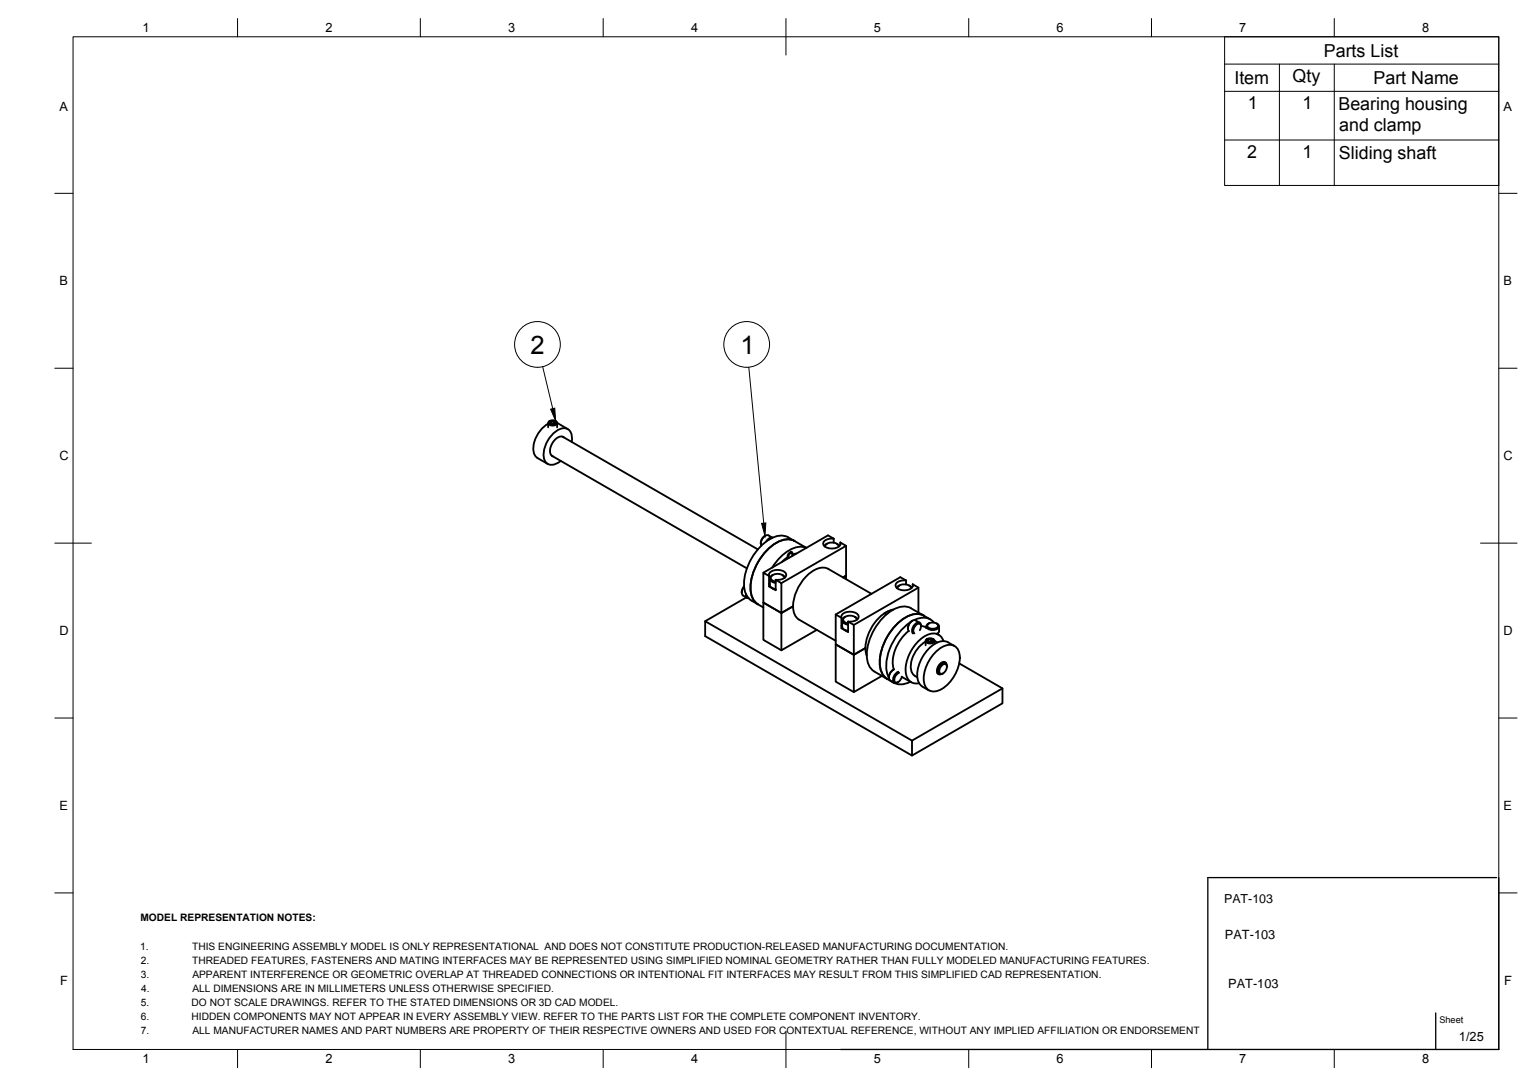
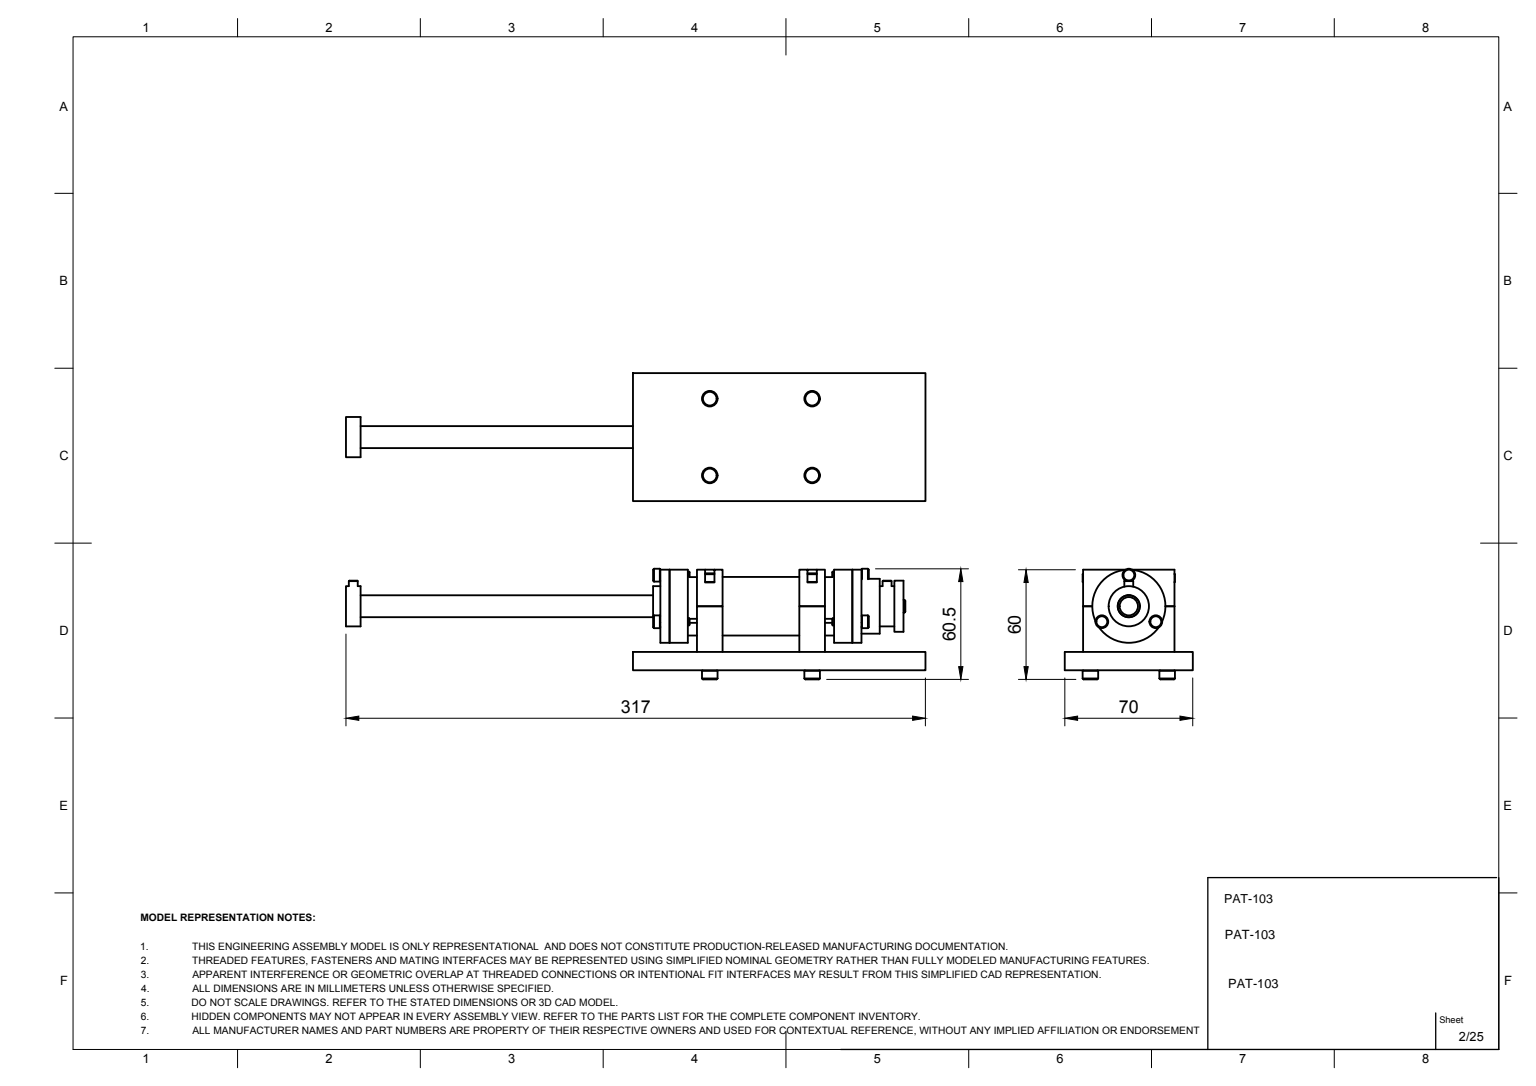
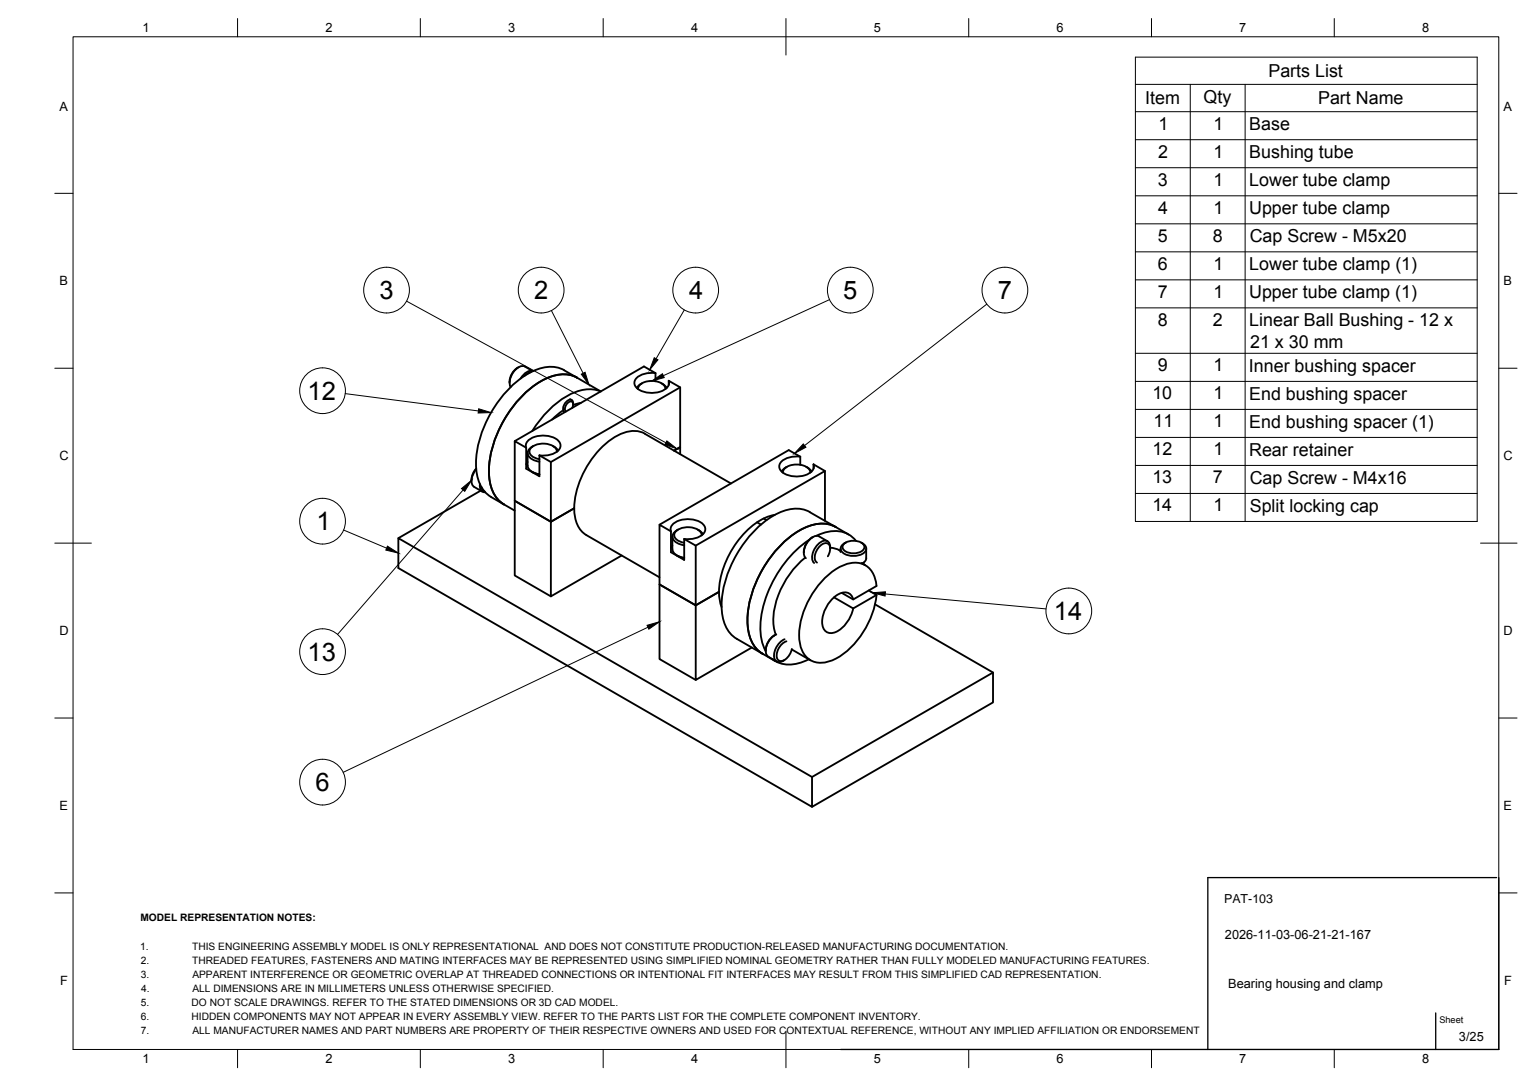
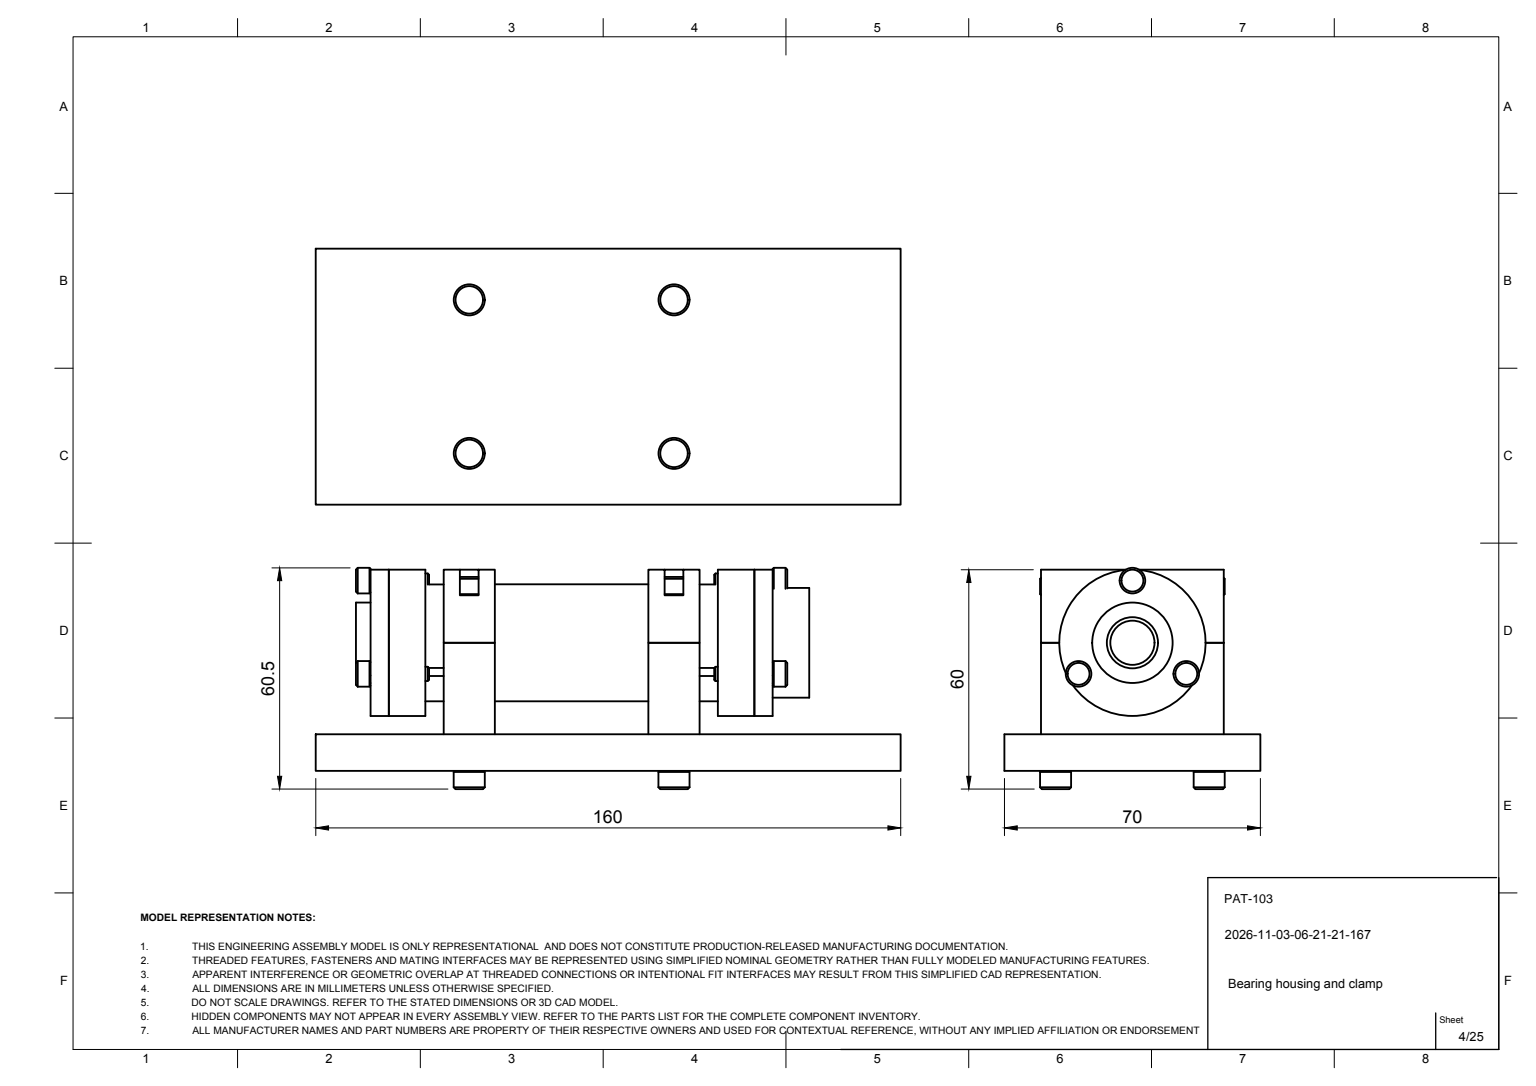
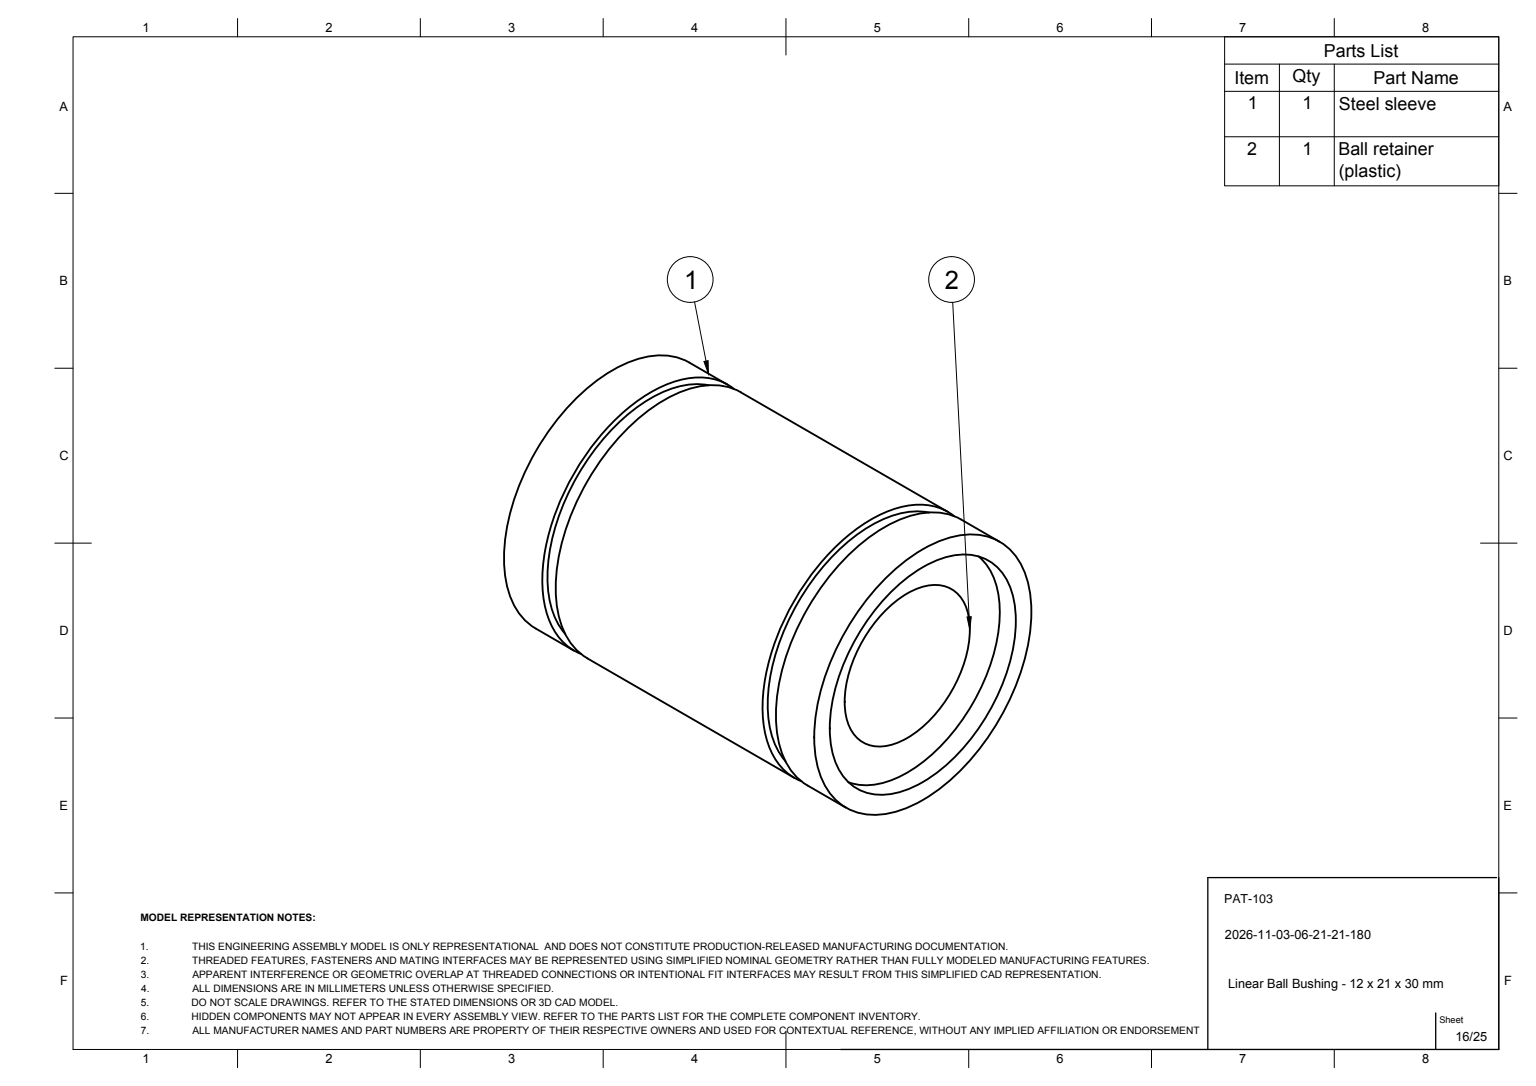
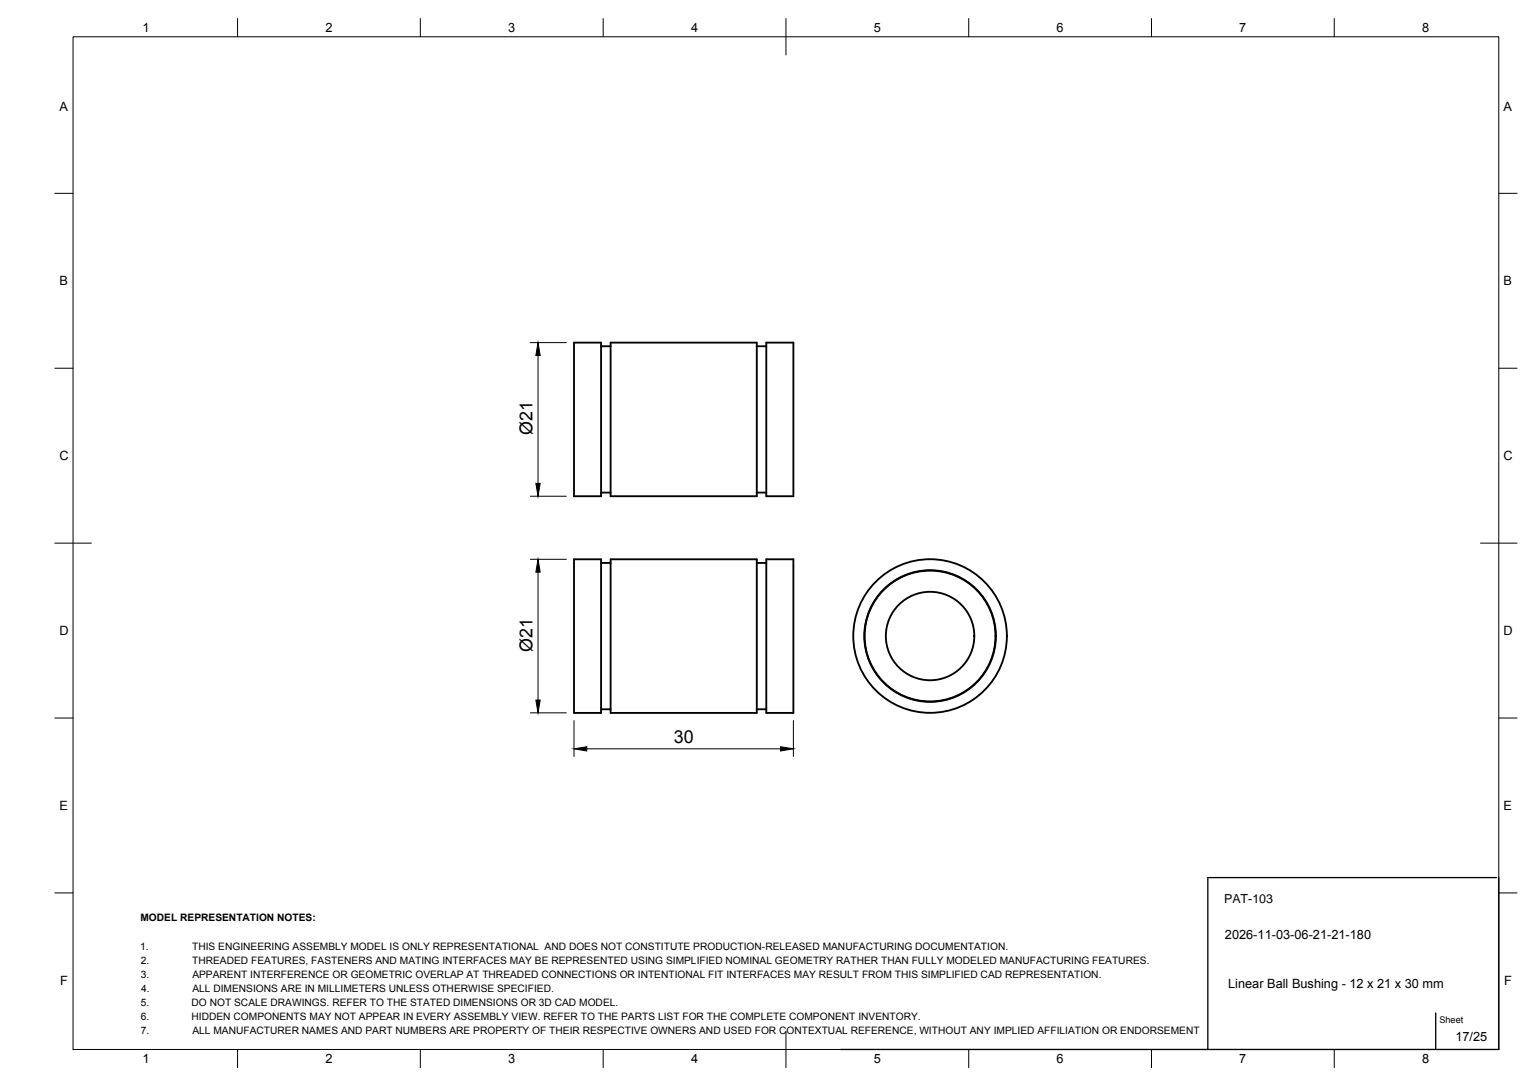
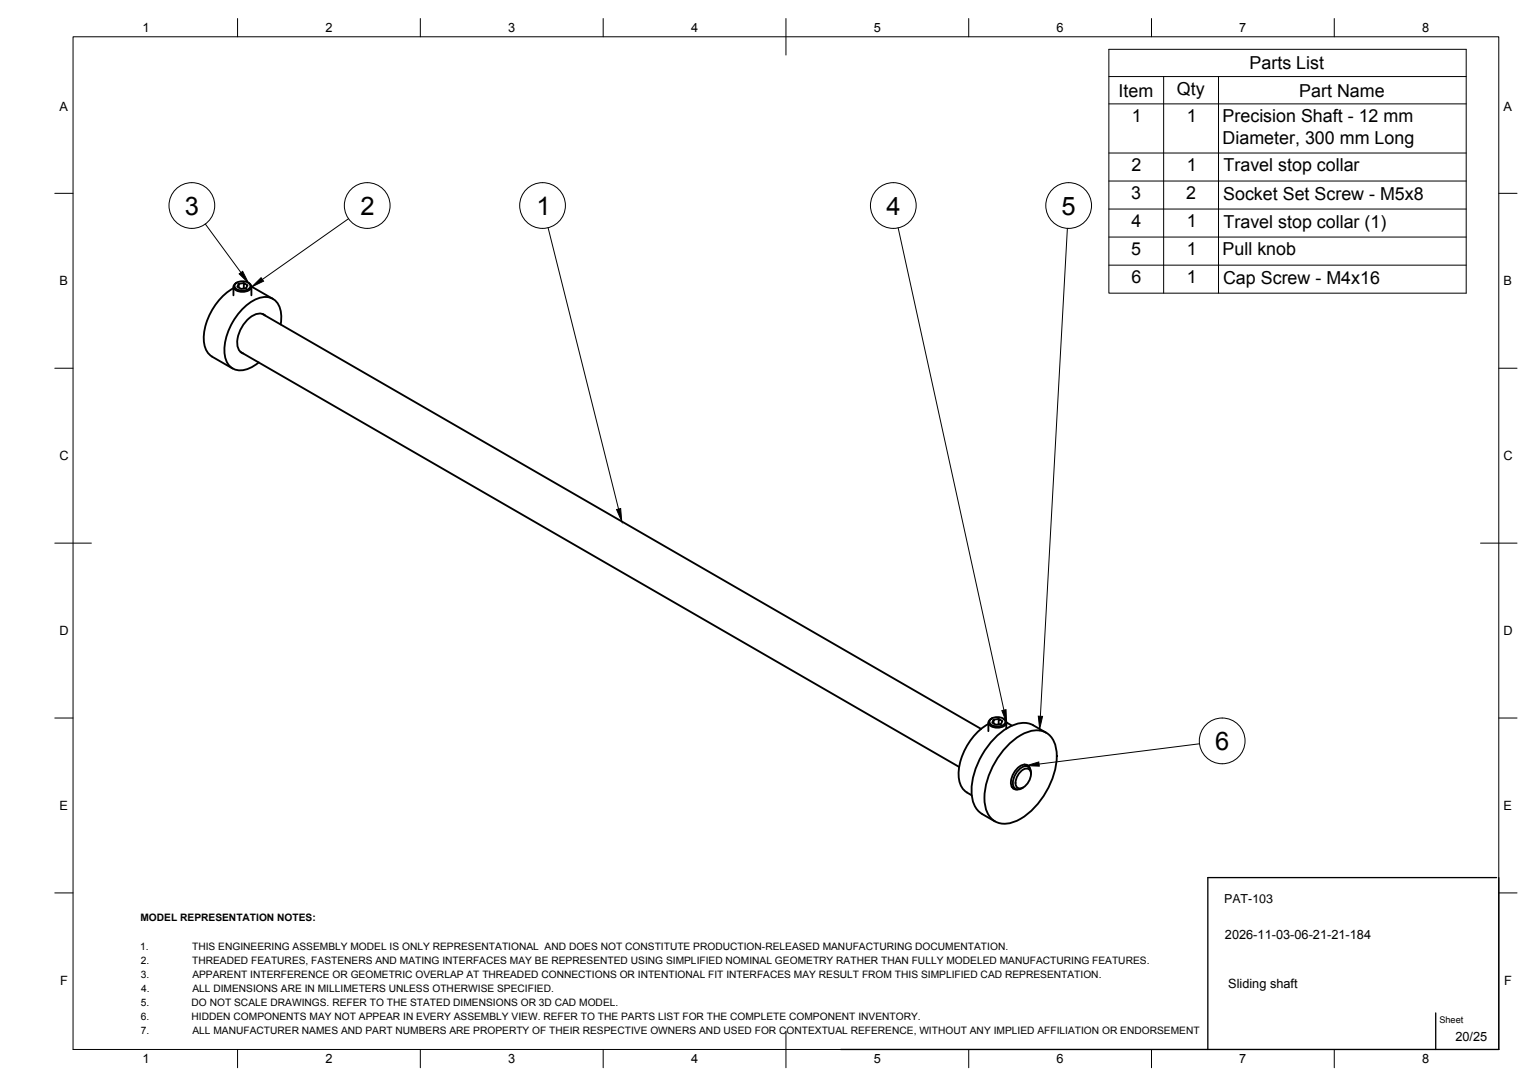
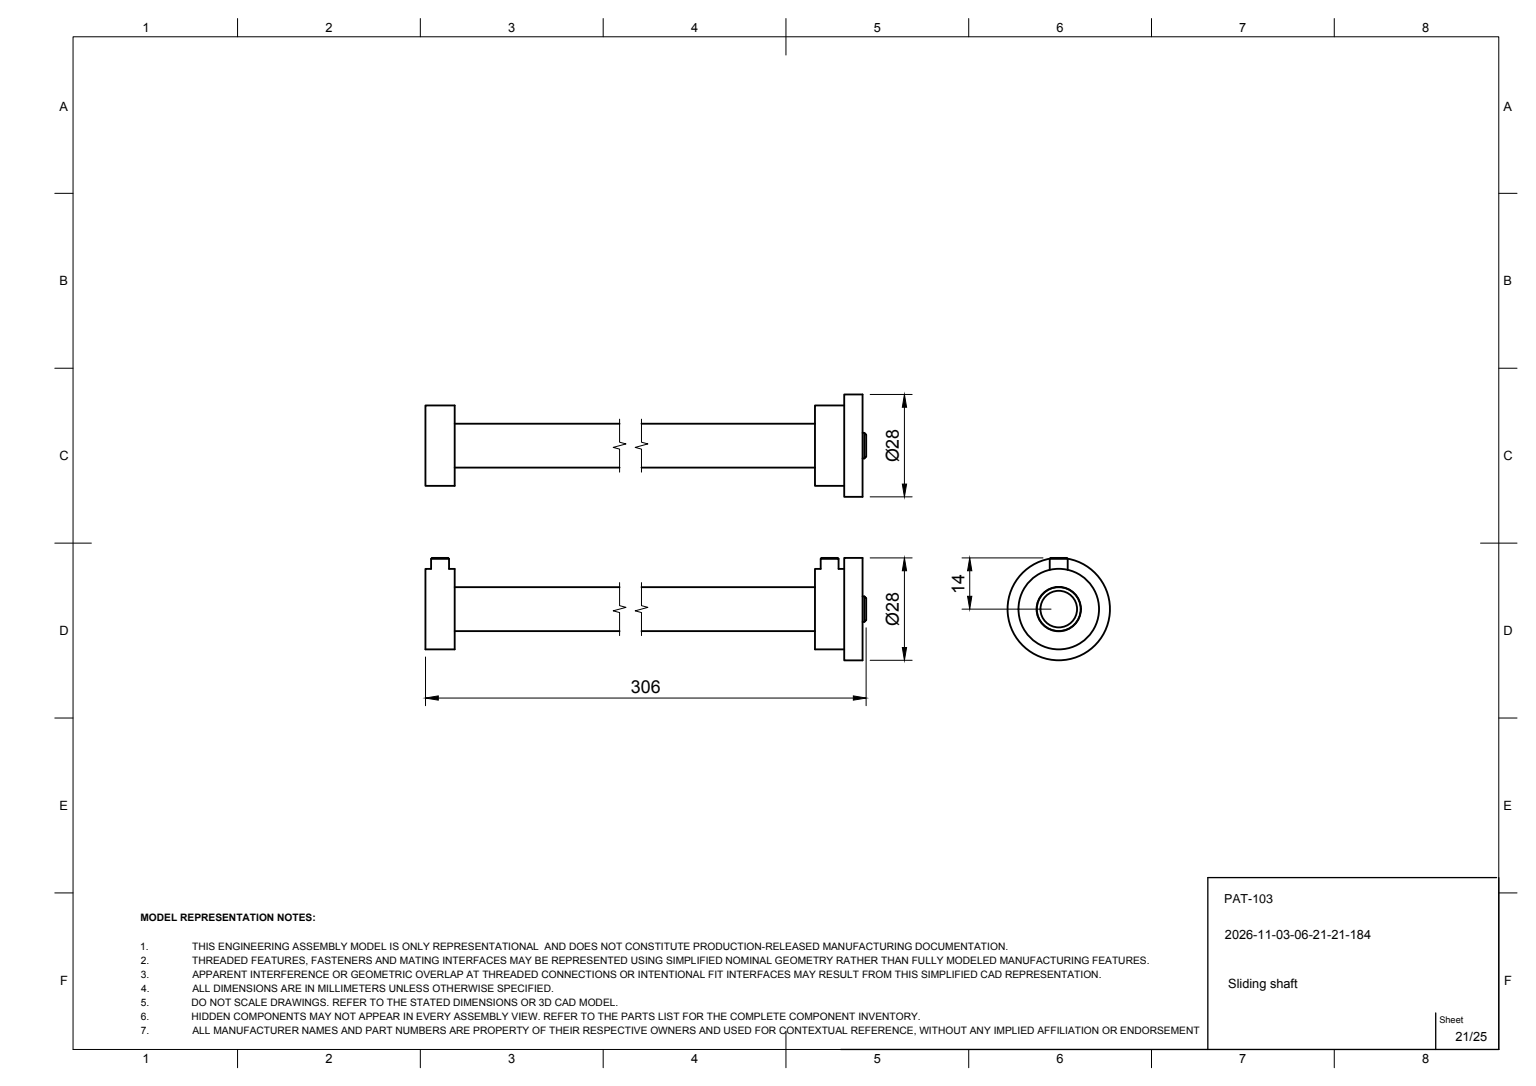
ISO-10303-21;
HEADER;
/* Generated by software containing ST-Developer
 * from STEP Tools, Inc. (www.steptools.com) 
 */

FILE_DESCRIPTION(
/* description */ ('Telescoping shaft support with lock collar'),
/* implementation_level */ '2;1');

FILE_NAME(
/* name */ 'PAT-103',
/* time_stamp */ '2026-10-27T10:48:51-07:00',
/* author */ (''),
/* organization */ (''),
/* preprocessor_version */ 'ST-DEVELOPER v20.2',
/* originating_system */ 'Autodesk Translation Framework v15.17.0.0',
/* authorisation */ '');

FILE_SCHEMA (('AUTOMOTIVE_DESIGN { 1 0 10303 214 3 1 1 }'));
ENDSEC;

DATA;
#10=MECHANICAL_DESIGN_GEOMETRIC_PRESENTATION_REPRESENTATION('',(#241,#242,
#243,#244,#245,#246,#247,#248,#249,#250,#251,#252,#253,#254,#255,#256,#257,
#258,#259,#260),#7349);
#11=ITEM_DEFINED_TRANSFORMATION($,$,#4520,#4569);
#12=ITEM_DEFINED_TRANSFORMATION($,$,#4552,#4570);
#13=ITEM_DEFINED_TRANSFORMATION($,$,#4209,#4670);
#14=ITEM_DEFINED_TRANSFORMATION($,$,#4228,#4671);
#15=ITEM_DEFINED_TRANSFORMATION($,$,#4293,#4672);
#16=ITEM_DEFINED_TRANSFORMATION($,$,#4320,#4673);
#17=ITEM_DEFINED_TRANSFORMATION($,$,#4345,#4674);
#18=ITEM_DEFINED_TRANSFORMATION($,$,#4372,#4675);
#19=ITEM_DEFINED_TRANSFORMATION($,$,#4397,#4676);
#20=ITEM_DEFINED_TRANSFORMATION($,$,#4406,#4677);
#21=ITEM_DEFINED_TRANSFORMATION($,$,#4415,#4678);
#22=ITEM_DEFINED_TRANSFORMATION($,$,#4424,#4679);
#23=ITEM_DEFINED_TRANSFORMATION($,$,#4446,#4680);
#24=ITEM_DEFINED_TRANSFORMATION($,$,#4493,#4681);
#25=ITEM_DEFINED_TRANSFORMATION($,$,#4493,#4682);
#26=ITEM_DEFINED_TRANSFORMATION($,$,#4493,#4683);
#27=ITEM_DEFINED_TRANSFORMATION($,$,#4493,#4684);
#28=ITEM_DEFINED_TRANSFORMATION($,$,#4493,#4685);
#29=ITEM_DEFINED_TRANSFORMATION($,$,#4493,#4686);
#30=ITEM_DEFINED_TRANSFORMATION($,$,#4493,#4687);
#31=ITEM_DEFINED_TRANSFORMATION($,$,#4493,#4688);
#32=ITEM_DEFINED_TRANSFORMATION($,$,#4519,#4689);
#33=ITEM_DEFINED_TRANSFORMATION($,$,#4519,#4690);
#34=ITEM_DEFINED_TRANSFORMATION($,$,#4644,#4691);
#35=ITEM_DEFINED_TRANSFORMATION($,$,#4644,#4692);
#36=ITEM_DEFINED_TRANSFORMATION($,$,#4644,#4693);
#37=ITEM_DEFINED_TRANSFORMATION($,$,#4644,#4694);
#38=ITEM_DEFINED_TRANSFORMATION($,$,#4644,#4695);
#39=ITEM_DEFINED_TRANSFORMATION($,$,#4644,#4696);
#40=ITEM_DEFINED_TRANSFORMATION($,$,#4644,#4697);
#41=ITEM_DEFINED_TRANSFORMATION($,$,#4572,#4698);
#42=ITEM_DEFINED_TRANSFORMATION($,$,#4586,#4699);
#43=ITEM_DEFINED_TRANSFORMATION($,$,#4600,#4700);
#44=ITEM_DEFINED_TRANSFORMATION($,$,#4613,#4701);
#45=ITEM_DEFINED_TRANSFORMATION($,$,#4627,#4702);
#46=ITEM_DEFINED_TRANSFORMATION($,$,#4627,#4703);
#47=ITEM_DEFINED_TRANSFORMATION($,$,#4644,#4704);
#48=ITEM_DEFINED_TRANSFORMATION($,$,#4208,#4705);
#49=ITEM_DEFINED_TRANSFORMATION($,$,#4571,#4706);
#50=(
REPRESENTATION_RELATIONSHIP($,$,#7456,#7455)
REPRESENTATION_RELATIONSHIP_WITH_TRANSFORMATION(#11)
SHAPE_REPRESENTATION_RELATIONSHIP()
);
#51=(
REPRESENTATION_RELATIONSHIP($,$,#7457,#7455)
REPRESENTATION_RELATIONSHIP_WITH_TRANSFORMATION(#12)
SHAPE_REPRESENTATION_RELATIONSHIP()
);
#52=(
REPRESENTATION_RELATIONSHIP($,$,#7443,#7442)
REPRESENTATION_RELATIONSHIP_WITH_TRANSFORMATION(#13)
SHAPE_REPRESENTATION_RELATIONSHIP()
);
#53=(
REPRESENTATION_RELATIONSHIP($,$,#7444,#7442)
REPRESENTATION_RELATIONSHIP_WITH_TRANSFORMATION(#14)
SHAPE_REPRESENTATION_RELATIONSHIP()
);
#54=(
REPRESENTATION_RELATIONSHIP($,$,#7445,#7442)
REPRESENTATION_RELATIONSHIP_WITH_TRANSFORMATION(#15)
SHAPE_REPRESENTATION_RELATIONSHIP()
);
#55=(
REPRESENTATION_RELATIONSHIP($,$,#7446,#7442)
REPRESENTATION_RELATIONSHIP_WITH_TRANSFORMATION(#16)
SHAPE_REPRESENTATION_RELATIONSHIP()
);
#56=(
REPRESENTATION_RELATIONSHIP($,$,#7447,#7442)
REPRESENTATION_RELATIONSHIP_WITH_TRANSFORMATION(#17)
SHAPE_REPRESENTATION_RELATIONSHIP()
);
#57=(
REPRESENTATION_RELATIONSHIP($,$,#7448,#7442)
REPRESENTATION_RELATIONSHIP_WITH_TRANSFORMATION(#18)
SHAPE_REPRESENTATION_RELATIONSHIP()
);
#58=(
REPRESENTATION_RELATIONSHIP($,$,#7449,#7442)
REPRESENTATION_RELATIONSHIP_WITH_TRANSFORMATION(#19)
SHAPE_REPRESENTATION_RELATIONSHIP()
);
#59=(
REPRESENTATION_RELATIONSHIP($,$,#7450,#7442)
REPRESENTATION_RELATIONSHIP_WITH_TRANSFORMATION(#20)
SHAPE_REPRESENTATION_RELATIONSHIP()
);
#60=(
REPRESENTATION_RELATIONSHIP($,$,#7451,#7442)
REPRESENTATION_RELATIONSHIP_WITH_TRANSFORMATION(#21)
SHAPE_REPRESENTATION_RELATIONSHIP()
);
#61=(
REPRESENTATION_RELATIONSHIP($,$,#7452,#7442)
REPRESENTATION_RELATIONSHIP_WITH_TRANSFORMATION(#22)
SHAPE_REPRESENTATION_RELATIONSHIP()
);
#62=(
REPRESENTATION_RELATIONSHIP($,$,#7453,#7442)
REPRESENTATION_RELATIONSHIP_WITH_TRANSFORMATION(#23)
SHAPE_REPRESENTATION_RELATIONSHIP()
);
#63=(
REPRESENTATION_RELATIONSHIP($,$,#7454,#7442)
REPRESENTATION_RELATIONSHIP_WITH_TRANSFORMATION(#24)
SHAPE_REPRESENTATION_RELATIONSHIP()
);
#64=(
REPRESENTATION_RELATIONSHIP($,$,#7454,#7442)
REPRESENTATION_RELATIONSHIP_WITH_TRANSFORMATION(#25)
SHAPE_REPRESENTATION_RELATIONSHIP()
);
#65=(
REPRESENTATION_RELATIONSHIP($,$,#7454,#7442)
REPRESENTATION_RELATIONSHIP_WITH_TRANSFORMATION(#26)
SHAPE_REPRESENTATION_RELATIONSHIP()
);
#66=(
REPRESENTATION_RELATIONSHIP($,$,#7454,#7442)
REPRESENTATION_RELATIONSHIP_WITH_TRANSFORMATION(#27)
SHAPE_REPRESENTATION_RELATIONSHIP()
);
#67=(
REPRESENTATION_RELATIONSHIP($,$,#7454,#7442)
REPRESENTATION_RELATIONSHIP_WITH_TRANSFORMATION(#28)
SHAPE_REPRESENTATION_RELATIONSHIP()
);
#68=(
REPRESENTATION_RELATIONSHIP($,$,#7454,#7442)
REPRESENTATION_RELATIONSHIP_WITH_TRANSFORMATION(#29)
SHAPE_REPRESENTATION_RELATIONSHIP()
);
#69=(
REPRESENTATION_RELATIONSHIP($,$,#7454,#7442)
REPRESENTATION_RELATIONSHIP_WITH_TRANSFORMATION(#30)
SHAPE_REPRESENTATION_RELATIONSHIP()
);
#70=(
REPRESENTATION_RELATIONSHIP($,$,#7454,#7442)
REPRESENTATION_RELATIONSHIP_WITH_TRANSFORMATION(#31)
SHAPE_REPRESENTATION_RELATIONSHIP()
);
#71=(
REPRESENTATION_RELATIONSHIP($,$,#7455,#7442)
REPRESENTATION_RELATIONSHIP_WITH_TRANSFORMATION(#32)
SHAPE_REPRESENTATION_RELATIONSHIP()
);
#72=(
REPRESENTATION_RELATIONSHIP($,$,#7455,#7442)
REPRESENTATION_RELATIONSHIP_WITH_TRANSFORMATION(#33)
SHAPE_REPRESENTATION_RELATIONSHIP()
);
#73=(
REPRESENTATION_RELATIONSHIP($,$,#7464,#7442)
REPRESENTATION_RELATIONSHIP_WITH_TRANSFORMATION(#34)
SHAPE_REPRESENTATION_RELATIONSHIP()
);
#74=(
REPRESENTATION_RELATIONSHIP($,$,#7464,#7442)
REPRESENTATION_RELATIONSHIP_WITH_TRANSFORMATION(#35)
SHAPE_REPRESENTATION_RELATIONSHIP()
);
#75=(
REPRESENTATION_RELATIONSHIP($,$,#7464,#7442)
REPRESENTATION_RELATIONSHIP_WITH_TRANSFORMATION(#36)
SHAPE_REPRESENTATION_RELATIONSHIP()
);
#76=(
REPRESENTATION_RELATIONSHIP($,$,#7464,#7442)
REPRESENTATION_RELATIONSHIP_WITH_TRANSFORMATION(#37)
SHAPE_REPRESENTATION_RELATIONSHIP()
);
#77=(
REPRESENTATION_RELATIONSHIP($,$,#7464,#7442)
REPRESENTATION_RELATIONSHIP_WITH_TRANSFORMATION(#38)
SHAPE_REPRESENTATION_RELATIONSHIP()
);
#78=(
REPRESENTATION_RELATIONSHIP($,$,#7464,#7442)
REPRESENTATION_RELATIONSHIP_WITH_TRANSFORMATION(#39)
SHAPE_REPRESENTATION_RELATIONSHIP()
);
#79=(
REPRESENTATION_RELATIONSHIP($,$,#7464,#7442)
REPRESENTATION_RELATIONSHIP_WITH_TRANSFORMATION(#40)
SHAPE_REPRESENTATION_RELATIONSHIP()
);
#80=(
REPRESENTATION_RELATIONSHIP($,$,#7459,#7458)
REPRESENTATION_RELATIONSHIP_WITH_TRANSFORMATION(#41)
SHAPE_REPRESENTATION_RELATIONSHIP()
);
#81=(
REPRESENTATION_RELATIONSHIP($,$,#7460,#7458)
REPRESENTATION_RELATIONSHIP_WITH_TRANSFORMATION(#42)
SHAPE_REPRESENTATION_RELATIONSHIP()
);
#82=(
REPRESENTATION_RELATIONSHIP($,$,#7461,#7458)
REPRESENTATION_RELATIONSHIP_WITH_TRANSFORMATION(#43)
SHAPE_REPRESENTATION_RELATIONSHIP()
);
#83=(
REPRESENTATION_RELATIONSHIP($,$,#7462,#7458)
REPRESENTATION_RELATIONSHIP_WITH_TRANSFORMATION(#44)
SHAPE_REPRESENTATION_RELATIONSHIP()
);
#84=(
REPRESENTATION_RELATIONSHIP($,$,#7463,#7458)
REPRESENTATION_RELATIONSHIP_WITH_TRANSFORMATION(#45)
SHAPE_REPRESENTATION_RELATIONSHIP()
);
#85=(
REPRESENTATION_RELATIONSHIP($,$,#7463,#7458)
REPRESENTATION_RELATIONSHIP_WITH_TRANSFORMATION(#46)
SHAPE_REPRESENTATION_RELATIONSHIP()
);
#86=(
REPRESENTATION_RELATIONSHIP($,$,#7464,#7458)
REPRESENTATION_RELATIONSHIP_WITH_TRANSFORMATION(#47)
SHAPE_REPRESENTATION_RELATIONSHIP()
);
#87=(
REPRESENTATION_RELATIONSHIP($,$,#7442,#7441)
REPRESENTATION_RELATIONSHIP_WITH_TRANSFORMATION(#48)
SHAPE_REPRESENTATION_RELATIONSHIP()
);
#88=(
REPRESENTATION_RELATIONSHIP($,$,#7458,#7441)
REPRESENTATION_RELATIONSHIP_WITH_TRANSFORMATION(#49)
SHAPE_REPRESENTATION_RELATIONSHIP()
);
#89=CONTEXT_DEPENDENT_SHAPE_REPRESENTATION(#50,#7395);
#90=CONTEXT_DEPENDENT_SHAPE_REPRESENTATION(#51,#7396);
#91=CONTEXT_DEPENDENT_SHAPE_REPRESENTATION(#52,#7404);
#92=CONTEXT_DEPENDENT_SHAPE_REPRESENTATION(#53,#7405);
#93=CONTEXT_DEPENDENT_SHAPE_REPRESENTATION(#54,#7406);
#94=CONTEXT_DEPENDENT_SHAPE_REPRESENTATION(#55,#7407);
#95=CONTEXT_DEPENDENT_SHAPE_REPRESENTATION(#56,#7408);
#96=CONTEXT_DEPENDENT_SHAPE_REPRESENTATION(#57,#7409);
#97=CONTEXT_DEPENDENT_SHAPE_REPRESENTATION(#58,#7410);
#98=CONTEXT_DEPENDENT_SHAPE_REPRESENTATION(#59,#7411);
#99=CONTEXT_DEPENDENT_SHAPE_REPRESENTATION(#60,#7412);
#100=CONTEXT_DEPENDENT_SHAPE_REPRESENTATION(#61,#7413);
#101=CONTEXT_DEPENDENT_SHAPE_REPRESENTATION(#62,#7414);
#102=CONTEXT_DEPENDENT_SHAPE_REPRESENTATION(#63,#7415);
#103=CONTEXT_DEPENDENT_SHAPE_REPRESENTATION(#64,#7416);
#104=CONTEXT_DEPENDENT_SHAPE_REPRESENTATION(#65,#7417);
#105=CONTEXT_DEPENDENT_SHAPE_REPRESENTATION(#66,#7418);
#106=CONTEXT_DEPENDENT_SHAPE_REPRESENTATION(#67,#7419);
#107=CONTEXT_DEPENDENT_SHAPE_REPRESENTATION(#68,#7420);
#108=CONTEXT_DEPENDENT_SHAPE_REPRESENTATION(#69,#7421);
#109=CONTEXT_DEPENDENT_SHAPE_REPRESENTATION(#70,#7422);
#110=CONTEXT_DEPENDENT_SHAPE_REPRESENTATION(#71,#7423);
#111=CONTEXT_DEPENDENT_SHAPE_REPRESENTATION(#72,#7424);
#112=CONTEXT_DEPENDENT_SHAPE_REPRESENTATION(#73,#7425);
#113=CONTEXT_DEPENDENT_SHAPE_REPRESENTATION(#74,#7426);
#114=CONTEXT_DEPENDENT_SHAPE_REPRESENTATION(#75,#7427);
#115=CONTEXT_DEPENDENT_SHAPE_REPRESENTATION(#76,#7428);
#116=CONTEXT_DEPENDENT_SHAPE_REPRESENTATION(#77,#7429);
#117=CONTEXT_DEPENDENT_SHAPE_REPRESENTATION(#78,#7430);
#118=CONTEXT_DEPENDENT_SHAPE_REPRESENTATION(#79,#7431);
#119=CONTEXT_DEPENDENT_SHAPE_REPRESENTATION(#80,#7432);
#120=CONTEXT_DEPENDENT_SHAPE_REPRESENTATION(#81,#7433);
#121=CONTEXT_DEPENDENT_SHAPE_REPRESENTATION(#82,#7434);
#122=CONTEXT_DEPENDENT_SHAPE_REPRESENTATION(#83,#7435);
#123=CONTEXT_DEPENDENT_SHAPE_REPRESENTATION(#84,#7436);
#124=CONTEXT_DEPENDENT_SHAPE_REPRESENTATION(#85,#7437);
#125=CONTEXT_DEPENDENT_SHAPE_REPRESENTATION(#86,#7438);
#126=CONTEXT_DEPENDENT_SHAPE_REPRESENTATION(#87,#7439);
#127=CONTEXT_DEPENDENT_SHAPE_REPRESENTATION(#88,#7440);
#128=NEXT_ASSEMBLY_USAGE_OCCURRENCE('Steel sleeve:1','Steel sleeve:1',
'Steel sleeve:1',#7480,#7481,'Steel sleeve:1');
#129=NEXT_ASSEMBLY_USAGE_OCCURRENCE('Ball retainer (plastic):1',
'Ball retainer (plastic):1','Ball retainer (plastic):1',#7480,#7482,
'Ball retainer (plastic):1');
#130=NEXT_ASSEMBLY_USAGE_OCCURRENCE('Base:1','Base:1','Base:1',#7467,#7468,
'Base:1');
#131=NEXT_ASSEMBLY_USAGE_OCCURRENCE('Bushing tube:1','Bushing tube:1',
'Bushing tube:1',#7467,#7469,'Bushing tube:1');
#132=NEXT_ASSEMBLY_USAGE_OCCURRENCE('Lower tube clamp:1',
'Lower tube clamp:1','Lower tube clamp:1',#7467,#7470,
'Lower tube clamp:1');
#133=NEXT_ASSEMBLY_USAGE_OCCURRENCE('Upper tube clamp:1',
'Upper tube clamp:1','Upper tube clamp:1',#7467,#7471,
'Upper tube clamp:1');
#134=NEXT_ASSEMBLY_USAGE_OCCURRENCE('Lower tube clamp (1):1',
'Lower tube clamp (1):1','Lower tube clamp (1):1',#7467,#7472,
'Lower tube clamp (1):1');
#135=NEXT_ASSEMBLY_USAGE_OCCURRENCE('Upper tube clamp (1):1',
'Upper tube clamp (1):1','Upper tube clamp (1):1',#7467,#7473,
'Upper tube clamp (1):1');
#136=NEXT_ASSEMBLY_USAGE_OCCURRENCE('Inner bushing spacer:1',
'Inner bushing spacer:1','Inner bushing spacer:1',#7467,#7474,
'Inner bushing spacer:1');
#137=NEXT_ASSEMBLY_USAGE_OCCURRENCE('End bushing spacer:1',
'End bushing spacer:1','End bushing spacer:1',#7467,#7475,
'End bushing spacer:1');
#138=NEXT_ASSEMBLY_USAGE_OCCURRENCE('End bushing spacer (1):1',
'End bushing spacer (1):1','End bushing spacer (1):1',#7467,#7476,
'End bushing spacer (1):1');
#139=NEXT_ASSEMBLY_USAGE_OCCURRENCE('Rear retainer:1','Rear retainer:1',
'Rear retainer:1',#7467,#7477,'Rear retainer:1');
#140=NEXT_ASSEMBLY_USAGE_OCCURRENCE('Split locking cap:1',
'Split locking cap:1','Split locking cap:1',#7467,#7478,
'Split locking cap:1');
#141=NEXT_ASSEMBLY_USAGE_OCCURRENCE('Cap Screw - M5x20:2',
'Cap Screw - M5x20:2','Cap Screw - M5x20:2',#7467,#7479,
'Cap Screw - M5x20:2');
#142=NEXT_ASSEMBLY_USAGE_OCCURRENCE('Cap Screw - M5x20:3',
'Cap Screw - M5x20:3','Cap Screw - M5x20:3',#7467,#7479,
'Cap Screw - M5x20:3');
#143=NEXT_ASSEMBLY_USAGE_OCCURRENCE('Cap Screw - M5x20:4',
'Cap Screw - M5x20:4','Cap Screw - M5x20:4',#7467,#7479,
'Cap Screw - M5x20:4');
#144=NEXT_ASSEMBLY_USAGE_OCCURRENCE('Cap Screw - M5x20:5',
'Cap Screw - M5x20:5','Cap Screw - M5x20:5',#7467,#7479,
'Cap Screw - M5x20:5');
#145=NEXT_ASSEMBLY_USAGE_OCCURRENCE('Cap Screw - M5x20:6',
'Cap Screw - M5x20:6','Cap Screw - M5x20:6',#7467,#7479,
'Cap Screw - M5x20:6');
#146=NEXT_ASSEMBLY_USAGE_OCCURRENCE('Cap Screw - M5x20:7',
'Cap Screw - M5x20:7','Cap Screw - M5x20:7',#7467,#7479,
'Cap Screw - M5x20:7');
#147=NEXT_ASSEMBLY_USAGE_OCCURRENCE('Cap Screw - M5x20:8',
'Cap Screw - M5x20:8','Cap Screw - M5x20:8',#7467,#7479,
'Cap Screw - M5x20:8');
#148=NEXT_ASSEMBLY_USAGE_OCCURRENCE('Cap Screw - M5x20:9',
'Cap Screw - M5x20:9','Cap Screw - M5x20:9',#7467,#7479,
'Cap Screw - M5x20:9');
#149=NEXT_ASSEMBLY_USAGE_OCCURRENCE(
'Linear Ball Bushing - 12 x 21 x 30 mm:2',
'Linear Ball Bushing - 12 x 21 x 30 mm:2',
'Linear Ball Bushing - 12 x 21 x 30 mm:2',#7467,#7480,
'Linear Ball Bushing - 12 x 21 x 30 mm:2');
#150=NEXT_ASSEMBLY_USAGE_OCCURRENCE(
'Linear Ball Bushing - 12 x 21 x 30 mm:3',
'Linear Ball Bushing - 12 x 21 x 30 mm:3',
'Linear Ball Bushing - 12 x 21 x 30 mm:3',#7467,#7480,
'Linear Ball Bushing - 12 x 21 x 30 mm:3');
#151=NEXT_ASSEMBLY_USAGE_OCCURRENCE('Cap Screw - M4x16:2',
'Cap Screw - M4x16:2','Cap Screw - M4x16:2',#7467,#7489,
'Cap Screw - M4x16:2');
#152=NEXT_ASSEMBLY_USAGE_OCCURRENCE('Cap Screw - M4x16:3',
'Cap Screw - M4x16:3','Cap Screw - M4x16:3',#7467,#7489,
'Cap Screw - M4x16:3');
#153=NEXT_ASSEMBLY_USAGE_OCCURRENCE('Cap Screw - M4x16:4',
'Cap Screw - M4x16:4','Cap Screw - M4x16:4',#7467,#7489,
'Cap Screw - M4x16:4');
#154=NEXT_ASSEMBLY_USAGE_OCCURRENCE('Cap Screw - M4x16:5',
'Cap Screw - M4x16:5','Cap Screw - M4x16:5',#7467,#7489,
'Cap Screw - M4x16:5');
#155=NEXT_ASSEMBLY_USAGE_OCCURRENCE('Cap Screw - M4x16:6',
'Cap Screw - M4x16:6','Cap Screw - M4x16:6',#7467,#7489,
'Cap Screw - M4x16:6');
#156=NEXT_ASSEMBLY_USAGE_OCCURRENCE('Cap Screw - M4x16:7',
'Cap Screw - M4x16:7','Cap Screw - M4x16:7',#7467,#7489,
'Cap Screw - M4x16:7');
#157=NEXT_ASSEMBLY_USAGE_OCCURRENCE('Cap Screw - M4x16:8',
'Cap Screw - M4x16:8','Cap Screw - M4x16:8',#7467,#7489,
'Cap Screw - M4x16:8');
#158=NEXT_ASSEMBLY_USAGE_OCCURRENCE('Travel stop collar:1',
'Travel stop collar:1','Travel stop collar:1',#7483,#7484,
'Travel stop collar:1');
#159=NEXT_ASSEMBLY_USAGE_OCCURRENCE('Travel stop collar (1):1',
'Travel stop collar (1):1','Travel stop collar (1):1',#7483,#7485,
'Travel stop collar (1):1');
#160=NEXT_ASSEMBLY_USAGE_OCCURRENCE('Pull knob:1','Pull knob:1',
'Pull knob:1',#7483,#7486,'Pull knob:1');
#161=NEXT_ASSEMBLY_USAGE_OCCURRENCE(
'Precision Shaft - 12 mm Diameter, 300 mm Long:2',
'Precision Shaft - 12 mm Diameter, 300 mm Long:2',
'Precision Shaft - 12 mm Diameter, 300 mm Long:2',#7483,#7487,
'Precision Shaft - 12 mm Diameter, 300 mm Long:2');
#162=NEXT_ASSEMBLY_USAGE_OCCURRENCE('Socket Set Screw - M5x8:2',
'Socket Set Screw - M5x8:2','Socket Set Screw - M5x8:2',#7483,#7488,
'Socket Set Screw - M5x8:2');
#163=NEXT_ASSEMBLY_USAGE_OCCURRENCE('Socket Set Screw - M5x8:3',
'Socket Set Screw - M5x8:3','Socket Set Screw - M5x8:3',#7483,#7488,
'Socket Set Screw - M5x8:3');
#164=NEXT_ASSEMBLY_USAGE_OCCURRENCE('Cap Screw - M4x16:9',
'Cap Screw - M4x16:9','Cap Screw - M4x16:9',#7483,#7489,
'Cap Screw - M4x16:9');
#165=NEXT_ASSEMBLY_USAGE_OCCURRENCE('Bearing housing and clamp:1',
'Bearing housing and clamp:1','Bearing housing and clamp:1',#7466,#7467,
'Bearing housing and clamp:1');
#166=NEXT_ASSEMBLY_USAGE_OCCURRENCE('Sliding shaft:1','Sliding shaft:1',
'Sliding shaft:1',#7466,#7483,'Sliding shaft:1');
#167=ORIENTED_CLOSED_SHELL('',*,#3976,.F.);
#168=ORIENTED_CLOSED_SHELL('',*,#3985,.F.);
#169=CONICAL_SURFACE('',#4496,0.4,0.785398163397448);
#170=CONICAL_SURFACE('',#4500,0.41,0.785398163397448);
#171=CONICAL_SURFACE('',#4504,0.26,0.463647609000806);
#172=CONICAL_SURFACE('',#4508,0.225,0.785398163397448);
#173=CONICAL_SURFACE('',#4618,0.55,0.785398163397448);
#174=CONICAL_SURFACE('',#4624,0.55,0.785398163397441);
#175=CONICAL_SURFACE('',#4637,0.235,0.785398163397448);
#176=CONICAL_SURFACE('',#4641,0.2125,0.785398163397448);
#177=CONICAL_SURFACE('',#4647,0.325,0.785398163397448);
#178=CONICAL_SURFACE('',#4651,0.335,0.785398163397448);
#179=CONICAL_SURFACE('',#4655,0.21,0.463647609000806);
#180=CONICAL_SURFACE('',#4659,0.18,0.785398163397448);
#181=BREP_WITH_VOIDS('Body1',#3975,(#167));
#182=BREP_WITH_VOIDS('Body1',#3984,(#168));
#183=B_SPLINE_CURVE_WITH_KNOTS('',3,(#6551,#6552,#6553,#6554,#6555,#6556,
#6557,#6558),.UNSPECIFIED.,.F.,.F.,(4,2,2,4),(0.211808182408868,0.240806862049815,
0.337801071942656,0.401300756844152),.UNSPECIFIED.);
#184=B_SPLINE_CURVE_WITH_KNOTS('',3,(#6559,#6560,#6561,#6562,#6563,#6564,
#6565,#6566,#6567,#6568,#6569,#6570,#6571,#6572,#6573,#6574,#6575,#6576,
#6577,#6578,#6579,#6580,#6581,#6582,#6583,#6584),.UNSPECIFIED.,.F.,.F.,
(4,2,2,2,2,2,2,2,2,2,2,2,4),(0.401300756844152,0.56115667536452,0.672834477075452,
0.784512278786384,0.830620394066968,0.876728509347553,0.922836624628137,
0.968944739908722,1.08062254161965,1.19230034333059,1.41565594675245,1.51265015664529,
1.54164883628624),.UNSPECIFIED.);
#185=B_SPLINE_CURVE_WITH_KNOTS('',3,(#6588,#6589,#6590,#6591,#6592,#6593,
#6594,#6595,#6596,#6597,#6598,#6599,#6600,#6601,#6602,#6603,#6604,#6605,
#6606,#6607,#6608,#6609,#6610,#6611,#6612,#6613,#6614,#6615,#6616,#6617),
 .UNSPECIFIED.,.F.,.F.,(4,2,2,2,2,2,2,2,2,2,2,2,2,2,4),(0.,0.0607190360347076,
0.121438072069415,0.209441873804407,0.2974456755394,0.399272742727807,0.501099809916215,
0.564787025689956,0.596630633576826,0.628474241463696,0.660317849350566,
0.692161457237437,0.755848673011177,0.857675740199585,0.959502807387993),
 .UNSPECIFIED.);
#186=B_SPLINE_CURVE_WITH_KNOTS('',3,(#6618,#6619,#6620,#6621,#6622,#6623,
#6624,#6625,#6626,#6627),.UNSPECIFIED.,.F.,.F.,(4,2,2,2,4),(0.959502807387993,
1.04750660912298,1.13551041085798,1.19622944689268,1.25694848292739),
 .UNSPECIFIED.);
#187=B_SPLINE_CURVE_WITH_KNOTS('',3,(#6910,#6911,#6912,#6913,#6914,#6915),
 .UNSPECIFIED.,.F.,.F.,(4,2,4),(0.818088904349175,0.878131747417171,0.957937926194042),
 .UNSPECIFIED.);
#188=B_SPLINE_CURVE_WITH_KNOTS('',3,(#6919,#6920,#6921,#6922,#6923,#6924),
 .UNSPECIFIED.,.F.,.F.,(4,2,4),(0.319312642064681,0.399118820841551,0.459161663909547),
 .UNSPECIFIED.);
#189=B_SPLINE_CURVE_WITH_KNOTS('',3,(#6925,#6926,#6927,#6928,#6929,#6930),
 .UNSPECIFIED.,.F.,.F.,(4,2,4),(0.179463620219814,0.23950646328781,0.319312642064681),
 .UNSPECIFIED.);
#190=B_SPLINE_CURVE_WITH_KNOTS('',3,(#6931,#6932,#6933,#6934,#6935,#6936),
 .UNSPECIFIED.,.F.,.F.,(4,2,4),(0.957937926194042,1.03774410497091,1.09778694803891),
 .UNSPECIFIED.);
#191=B_SPLINE_CURVE_WITH_KNOTS('',3,(#6940,#6941,#6942,#6943,#6944,#6945,
#6946,#6947,#6948,#6949),.UNSPECIFIED.,.F.,.F.,(4,2,2,2,4),(0.,0.0793157643915228,
0.158631528783046,0.237943615933651,0.317255703084257),.UNSPECIFIED.);
#192=B_SPLINE_CURVE_WITH_KNOTS('',3,(#6951,#6952,#6953,#6954,#6955,#6956,
#6957,#6958,#6959,#6960),.UNSPECIFIED.,.F.,.F.,(4,2,2,2,4),(0.951767109252772,
1.03107919640338,1.11039128355398,1.18970704794551,1.26902281233703),
 .UNSPECIFIED.);
#193=B_SPLINE_CURVE_WITH_KNOTS('',3,(#6961,#6962,#6963,#6964,#6965,#6966,
#6967,#6968,#6969,#6970,#6971,#6972,#6973,#6974,#6975,#6976,#6977,#6978),
 .UNSPECIFIED.,.F.,.F.,(4,2,2,2,2,2,2,2,4),(0.317255703084257,0.396567790234863,
0.475879877385469,0.555195641776992,0.634511406168514,0.713827170560037,
0.79314293495156,0.872455022102166,0.951767109252772),.UNSPECIFIED.);
#194=B_SPLINE_CURVE_WITH_KNOTS('',3,(#7006,#7007,#7008,#7009,#7010,#7011),
 .UNSPECIFIED.,.F.,.F.,(4,2,4),(0.81808890434917,0.878131747417167,0.957937926194039),
 .UNSPECIFIED.);
#195=B_SPLINE_CURVE_WITH_KNOTS('',3,(#7015,#7016,#7017,#7018,#7019,#7020),
 .UNSPECIFIED.,.F.,.F.,(4,2,4),(0.31931264206468,0.399118820841551,0.459161663909546),
 .UNSPECIFIED.);
#196=B_SPLINE_CURVE_WITH_KNOTS('',3,(#7021,#7022,#7023,#7024,#7025,#7026),
 .UNSPECIFIED.,.F.,.F.,(4,2,4),(0.179463620219813,0.239506463287808,0.31931264206468),
 .UNSPECIFIED.);
#197=B_SPLINE_CURVE_WITH_KNOTS('',3,(#7027,#7028,#7029,#7030,#7031,#7032),
 .UNSPECIFIED.,.F.,.F.,(4,2,4),(0.957937926194039,1.03774410497091,1.09778694803891),
 .UNSPECIFIED.);
#198=B_SPLINE_CURVE_WITH_KNOTS('',3,(#7036,#7037,#7038,#7039,#7040,#7041,
#7042,#7043,#7044,#7045),.UNSPECIFIED.,.F.,.F.,(4,2,2,2,4),(0.,0.0793157643915219,
0.158631528783044,0.23794361593365,0.317255703084256),.UNSPECIFIED.);
#199=B_SPLINE_CURVE_WITH_KNOTS('',3,(#7047,#7048,#7049,#7050,#7051,#7052,
#7053,#7054,#7055,#7056),.UNSPECIFIED.,.F.,.F.,(4,2,2,2,4),(0.951767109252769,
1.03107919640337,1.11039128355398,1.1897070479455,1.26902281233703),
 .UNSPECIFIED.);
#200=B_SPLINE_CURVE_WITH_KNOTS('',3,(#7057,#7058,#7059,#7060,#7061,#7062,
#7063,#7064,#7065,#7066,#7067,#7068,#7069,#7070,#7071,#7072,#7073,#7074),
 .UNSPECIFIED.,.F.,.F.,(4,2,2,2,2,2,2,2,4),(0.317255703084256,0.396567790234863,
0.475879877385469,0.555195641776991,0.634511406168513,0.713827170560035,
0.793142934951556,0.872455022102163,0.951767109252769),.UNSPECIFIED.);
#201=SHAPE_REPRESENTATION_RELATIONSHIP('SRR','None',#7443,#221);
#202=SHAPE_REPRESENTATION_RELATIONSHIP('SRR','None',#7444,#222);
#203=SHAPE_REPRESENTATION_RELATIONSHIP('SRR','None',#7445,#223);
#204=SHAPE_REPRESENTATION_RELATIONSHIP('SRR','None',#7446,#224);
#205=SHAPE_REPRESENTATION_RELATIONSHIP('SRR','None',#7447,#225);
#206=SHAPE_REPRESENTATION_RELATIONSHIP('SRR','None',#7448,#226);
#207=SHAPE_REPRESENTATION_RELATIONSHIP('SRR','None',#7449,#227);
#208=SHAPE_REPRESENTATION_RELATIONSHIP('SRR','None',#7450,#228);
#209=SHAPE_REPRESENTATION_RELATIONSHIP('SRR','None',#7451,#229);
#210=SHAPE_REPRESENTATION_RELATIONSHIP('SRR','None',#7452,#230);
#211=SHAPE_REPRESENTATION_RELATIONSHIP('SRR','None',#7453,#231);
#212=SHAPE_REPRESENTATION_RELATIONSHIP('SRR','None',#7454,#232);
#213=SHAPE_REPRESENTATION_RELATIONSHIP('SRR','None',#7456,#233);
#214=SHAPE_REPRESENTATION_RELATIONSHIP('SRR','None',#7457,#234);
#215=SHAPE_REPRESENTATION_RELATIONSHIP('SRR','None',#7459,#235);
#216=SHAPE_REPRESENTATION_RELATIONSHIP('SRR','None',#7460,#236);
#217=SHAPE_REPRESENTATION_RELATIONSHIP('SRR','None',#7461,#237);
#218=SHAPE_REPRESENTATION_RELATIONSHIP('SRR','None',#7462,#238);
#219=SHAPE_REPRESENTATION_RELATIONSHIP('SRR','None',#7463,#239);
#220=SHAPE_REPRESENTATION_RELATIONSHIP('SRR','None',#7464,#240);
#221=ADVANCED_BREP_SHAPE_REPRESENTATION('',(#261),#7327);
#222=ADVANCED_BREP_SHAPE_REPRESENTATION('',(#262),#7328);
#223=ADVANCED_BREP_SHAPE_REPRESENTATION('',(#263),#7329);
#224=ADVANCED_BREP_SHAPE_REPRESENTATION('',(#264),#7330);
#225=ADVANCED_BREP_SHAPE_REPRESENTATION('',(#265),#7331);
#226=ADVANCED_BREP_SHAPE_REPRESENTATION('',(#266),#7332);
#227=ADVANCED_BREP_SHAPE_REPRESENTATION('',(#267),#7333);
#228=ADVANCED_BREP_SHAPE_REPRESENTATION('',(#268),#7334);
#229=ADVANCED_BREP_SHAPE_REPRESENTATION('',(#269),#7335);
#230=ADVANCED_BREP_SHAPE_REPRESENTATION('',(#270),#7336);
#231=ADVANCED_BREP_SHAPE_REPRESENTATION('',(#271),#7337);
#232=ADVANCED_BREP_SHAPE_REPRESENTATION('',(#181),#7338);
#233=ADVANCED_BREP_SHAPE_REPRESENTATION('',(#272),#7340);
#234=ADVANCED_BREP_SHAPE_REPRESENTATION('',(#273),#7341);
#235=ADVANCED_BREP_SHAPE_REPRESENTATION('',(#274),#7343);
#236=ADVANCED_BREP_SHAPE_REPRESENTATION('',(#275),#7344);
#237=ADVANCED_BREP_SHAPE_REPRESENTATION('',(#276),#7345);
#238=ADVANCED_BREP_SHAPE_REPRESENTATION('',(#277),#7346);
#239=ADVANCED_BREP_SHAPE_REPRESENTATION('',(#278),#7347);
#240=ADVANCED_BREP_SHAPE_REPRESENTATION('',(#182),#7348);
#241=STYLED_ITEM('',(#7606),#261);
#242=STYLED_ITEM('',(#7641),#262);
#243=STYLED_ITEM('',(#7613),#263);
#244=STYLED_ITEM('',(#7641),#264);
#245=STYLED_ITEM('',(#7613),#265);
#246=STYLED_ITEM('',(#7641),#266);
#247=STYLED_ITEM('',(#7620),#267);
#248=STYLED_ITEM('',(#7641),#268);
#249=STYLED_ITEM('',(#7641),#269);
#250=STYLED_ITEM('',(#7620),#270);
#251=STYLED_ITEM('',(#7620),#271);
#252=STYLED_ITEM('',(#7634),#181);
#253=STYLED_ITEM('',(#7641),#272);
#254=STYLED_ITEM('',(#7620),#273);
#255=STYLED_ITEM('',(#7641),#274);
#256=STYLED_ITEM('',(#7641),#275);
#257=STYLED_ITEM('',(#7620),#276);
#258=STYLED_ITEM('',(#7627),#277);
#259=STYLED_ITEM('',(#7634),#278);
#260=STYLED_ITEM('',(#7634),#182);
#261=MANIFOLD_SOLID_BREP('Body1',#3964);
#262=MANIFOLD_SOLID_BREP('Body1',#3965);
#263=MANIFOLD_SOLID_BREP('Body1',#3966);
#264=MANIFOLD_SOLID_BREP('Body1',#3967);
#265=MANIFOLD_SOLID_BREP('Body1',#3968);
#266=MANIFOLD_SOLID_BREP('Body1',#3969);
#267=MANIFOLD_SOLID_BREP('Body1',#3970);
#268=MANIFOLD_SOLID_BREP('Body1',#3971);
#269=MANIFOLD_SOLID_BREP('Body1',#3972);
#270=MANIFOLD_SOLID_BREP('Body1',#3973);
#271=MANIFOLD_SOLID_BREP('Body1',#3974);
#272=MANIFOLD_SOLID_BREP('Body1',#3977);
#273=MANIFOLD_SOLID_BREP('Body1',#3978);
#274=MANIFOLD_SOLID_BREP('Body1',#3979);
#275=MANIFOLD_SOLID_BREP('Body1',#3980);
#276=MANIFOLD_SOLID_BREP('Body1',#3981);
#277=MANIFOLD_SOLID_BREP('Body1',#3982);
#278=MANIFOLD_SOLID_BREP('Body1',#3983);
#279=FACE_BOUND('',#730,.T.);
#280=FACE_BOUND('',#731,.T.);
#281=FACE_BOUND('',#732,.T.);
#282=FACE_BOUND('',#733,.T.);
#283=FACE_BOUND('',#735,.T.);
#284=FACE_BOUND('',#736,.T.);
#285=FACE_BOUND('',#737,.T.);
#286=FACE_BOUND('',#738,.T.);
#287=FACE_BOUND('',#746,.T.);
#288=FACE_BOUND('',#756,.T.);
#289=FACE_BOUND('',#760,.T.);
#290=FACE_BOUND('',#761,.T.);
#291=FACE_BOUND('',#762,.T.);
#292=FACE_BOUND('',#763,.T.);
#293=FACE_BOUND('',#765,.T.);
#294=FACE_BOUND('',#766,.T.);
#295=FACE_BOUND('',#767,.T.);
#296=FACE_BOUND('',#768,.T.);
#297=FACE_BOUND('',#780,.T.);
#298=FACE_BOUND('',#785,.T.);
#299=FACE_BOUND('',#787,.T.);
#300=FACE_BOUND('',#788,.T.);
#301=FACE_BOUND('',#790,.T.);
#302=FACE_BOUND('',#793,.T.);
#303=FACE_BOUND('',#802,.T.);
#304=FACE_BOUND('',#806,.T.);
#305=FACE_BOUND('',#818,.T.);
#306=FACE_BOUND('',#823,.T.);
#307=FACE_BOUND('',#825,.T.);
#308=FACE_BOUND('',#826,.T.);
#309=FACE_BOUND('',#828,.T.);
#310=FACE_BOUND('',#831,.T.);
#311=FACE_BOUND('',#840,.T.);
#312=FACE_BOUND('',#844,.T.);
#313=FACE_BOUND('',#848,.T.);
#314=FACE_BOUND('',#850,.T.);
#315=FACE_BOUND('',#854,.T.);
#316=FACE_BOUND('',#856,.T.);
#317=FACE_BOUND('',#860,.T.);
#318=FACE_BOUND('',#862,.T.);
#319=FACE_BOUND('',#868,.T.);
#320=FACE_BOUND('',#872,.T.);
#321=FACE_BOUND('',#873,.T.);
#322=FACE_BOUND('',#874,.T.);
#323=FACE_BOUND('',#875,.T.);
#324=FACE_BOUND('',#877,.T.);
#325=FACE_BOUND('',#878,.T.);
#326=FACE_BOUND('',#879,.T.);
#327=FACE_BOUND('',#880,.T.);
#328=FACE_BOUND('',#891,.T.);
#329=FACE_BOUND('',#892,.T.);
#330=FACE_BOUND('',#894,.T.);
#331=FACE_BOUND('',#896,.T.);
#332=FACE_BOUND('',#898,.T.);
#333=FACE_BOUND('',#903,.T.);
#334=FACE_BOUND('',#904,.T.);
#335=FACE_BOUND('',#905,.T.);
#336=FACE_BOUND('',#906,.T.);
#337=FACE_BOUND('',#912,.T.);
#338=FACE_BOUND('',#931,.T.);
#339=FACE_BOUND('',#934,.T.);
#340=FACE_BOUND('',#937,.T.);
#341=FACE_BOUND('',#940,.T.);
#342=FACE_BOUND('',#943,.T.);
#343=FACE_BOUND('',#946,.T.);
#344=FACE_BOUND('',#948,.T.);
#345=FACE_BOUND('',#954,.T.);
#346=FACE_BOUND('',#956,.T.);
#347=FACE_BOUND('',#958,.T.);
#348=FACE_BOUND('',#960,.T.);
#349=FACE_BOUND('',#967,.T.);
#350=FACE_BOUND('',#969,.T.);
#351=FACE_BOUND('',#976,.T.);
#352=FACE_BOUND('',#978,.T.);
#353=FACE_BOUND('',#981,.T.);
#354=FACE_BOUND('',#985,.T.);
#355=FACE_BOUND('',#987,.T.);
#356=FACE_BOUND('',#995,.T.);
#357=FACE_BOUND('',#1004,.T.);
#358=FACE_BOUND('',#1014,.T.);
#359=PLANE('',#4222);
#360=PLANE('',#4223);
#361=PLANE('',#4224);
#362=PLANE('',#4225);
#363=PLANE('',#4226);
#364=PLANE('',#4227);
#365=PLANE('',#4234);
#366=PLANE('',#4242);
#367=PLANE('',#4249);
#368=PLANE('',#4251);
#369=PLANE('',#4256);
#370=PLANE('',#4264);
#371=PLANE('',#4271);
#372=PLANE('',#4284);
#373=PLANE('',#4291);
#374=PLANE('',#4292);
#375=PLANE('',#4297);
#376=PLANE('',#4301);
#377=PLANE('',#4305);
#378=PLANE('',#4309);
#379=PLANE('',#4313);
#380=PLANE('',#4314);
#381=PLANE('',#4315);
#382=PLANE('',#4316);
#383=PLANE('',#4317);
#384=PLANE('',#4318);
#385=PLANE('',#4319);
#386=PLANE('',#4321);
#387=PLANE('',#4326);
#388=PLANE('',#4331);
#389=PLANE('',#4332);
#390=PLANE('',#4340);
#391=PLANE('',#4341);
#392=PLANE('',#4342);
#393=PLANE('',#4343);
#394=PLANE('',#4344);
#395=PLANE('',#4349);
#396=PLANE('',#4353);
#397=PLANE('',#4357);
#398=PLANE('',#4361);
#399=PLANE('',#4365);
#400=PLANE('',#4366);
#401=PLANE('',#4367);
#402=PLANE('',#4368);
#403=PLANE('',#4369);
#404=PLANE('',#4370);
#405=PLANE('',#4371);
#406=PLANE('',#4373);
#407=PLANE('',#4378);
#408=PLANE('',#4383);
#409=PLANE('',#4384);
#410=PLANE('',#4392);
#411=PLANE('',#4393);
#412=PLANE('',#4394);
#413=PLANE('',#4395);
#414=PLANE('',#4396);
#415=PLANE('',#4404);
#416=PLANE('',#4405);
#417=PLANE('',#4413);
#418=PLANE('',#4414);
#419=PLANE('',#4422);
#420=PLANE('',#4423);
#421=PLANE('',#4437);
#422=PLANE('',#4444);
#423=PLANE('',#4445);
#424=PLANE('',#4447);
#425=PLANE('',#4453);
#426=PLANE('',#4460);
#427=PLANE('',#4467);
#428=PLANE('',#4480);
#429=PLANE('',#4481);
#430=PLANE('',#4482);
#431=PLANE('',#4485);
#432=PLANE('',#4492);
#433=PLANE('',#4494);
#434=PLANE('',#4502);
#435=PLANE('',#4510);
#436=PLANE('',#4511);
#437=PLANE('',#4512);
#438=PLANE('',#4513);
#439=PLANE('',#4514);
#440=PLANE('',#4515);
#441=PLANE('',#4516);
#442=PLANE('',#4517);
#443=PLANE('',#4518);
#444=PLANE('',#4521);
#445=PLANE('',#4523);
#446=PLANE('',#4524);
#447=PLANE('',#4526);
#448=PLANE('',#4527);
#449=PLANE('',#4528);
#450=PLANE('',#4533);
#451=PLANE('',#4537);
#452=PLANE('',#4541);
#453=PLANE('',#4545);
#454=PLANE('',#4549);
#455=PLANE('',#4553);
#456=PLANE('',#4556);
#457=PLANE('',#4557);
#458=PLANE('',#4560);
#459=PLANE('',#4561);
#460=PLANE('',#4566);
#461=PLANE('',#4573);
#462=PLANE('',#4577);
#463=PLANE('',#4584);
#464=PLANE('',#4585);
#465=PLANE('',#4587);
#466=PLANE('',#4591);
#467=PLANE('',#4598);
#468=PLANE('',#4599);
#469=PLANE('',#4604);
#470=PLANE('',#4611);
#471=PLANE('',#4612);
#472=PLANE('',#4617);
#473=PLANE('',#4623);
#474=PLANE('',#4626);
#475=PLANE('',#4628);
#476=PLANE('',#4629);
#477=PLANE('',#4630);
#478=PLANE('',#4631);
#479=PLANE('',#4632);
#480=PLANE('',#4633);
#481=PLANE('',#4634);
#482=PLANE('',#4635);
#483=PLANE('',#4643);
#484=PLANE('',#4645);
#485=PLANE('',#4653);
#486=PLANE('',#4661);
#487=PLANE('',#4662);
#488=PLANE('',#4663);
#489=PLANE('',#4664);
#490=PLANE('',#4665);
#491=PLANE('',#4666);
#492=PLANE('',#4667);
#493=PLANE('',#4668);
#494=PLANE('',#4669);
#495=FACE_OUTER_BOUND('',#721,.T.);
#496=FACE_OUTER_BOUND('',#722,.T.);
#497=FACE_OUTER_BOUND('',#723,.T.);
#498=FACE_OUTER_BOUND('',#724,.T.);
#499=FACE_OUTER_BOUND('',#725,.T.);
#500=FACE_OUTER_BOUND('',#726,.T.);
#501=FACE_OUTER_BOUND('',#727,.T.);
#502=FACE_OUTER_BOUND('',#728,.T.);
#503=FACE_OUTER_BOUND('',#729,.T.);
#504=FACE_OUTER_BOUND('',#734,.T.);
#505=FACE_OUTER_BOUND('',#739,.T.);
#506=FACE_OUTER_BOUND('',#740,.T.);
#507=FACE_OUTER_BOUND('',#741,.T.);
#508=FACE_OUTER_BOUND('',#742,.T.);
#509=FACE_OUTER_BOUND('',#743,.T.);
#510=FACE_OUTER_BOUND('',#744,.T.);
#511=FACE_OUTER_BOUND('',#745,.T.);
#512=FACE_OUTER_BOUND('',#747,.T.);
#513=FACE_OUTER_BOUND('',#748,.T.);
#514=FACE_OUTER_BOUND('',#749,.T.);
#515=FACE_OUTER_BOUND('',#750,.T.);
#516=FACE_OUTER_BOUND('',#751,.T.);
#517=FACE_OUTER_BOUND('',#752,.T.);
#518=FACE_OUTER_BOUND('',#753,.T.);
#519=FACE_OUTER_BOUND('',#754,.T.);
#520=FACE_OUTER_BOUND('',#755,.T.);
#521=FACE_OUTER_BOUND('',#757,.T.);
#522=FACE_OUTER_BOUND('',#758,.T.);
#523=FACE_OUTER_BOUND('',#759,.T.);
#524=FACE_OUTER_BOUND('',#764,.T.);
#525=FACE_OUTER_BOUND('',#769,.T.);
#526=FACE_OUTER_BOUND('',#770,.T.);
#527=FACE_OUTER_BOUND('',#771,.T.);
#528=FACE_OUTER_BOUND('',#772,.T.);
#529=FACE_OUTER_BOUND('',#773,.T.);
#530=FACE_OUTER_BOUND('',#774,.T.);
#531=FACE_OUTER_BOUND('',#775,.T.);
#532=FACE_OUTER_BOUND('',#776,.T.);
#533=FACE_OUTER_BOUND('',#777,.T.);
#534=FACE_OUTER_BOUND('',#778,.T.);
#535=FACE_OUTER_BOUND('',#779,.T.);
#536=FACE_OUTER_BOUND('',#781,.T.);
#537=FACE_OUTER_BOUND('',#782,.T.);
#538=FACE_OUTER_BOUND('',#783,.T.);
#539=FACE_OUTER_BOUND('',#784,.T.);
#540=FACE_OUTER_BOUND('',#786,.T.);
#541=FACE_OUTER_BOUND('',#789,.T.);
#542=FACE_OUTER_BOUND('',#791,.T.);
#543=FACE_OUTER_BOUND('',#792,.T.);
#544=FACE_OUTER_BOUND('',#794,.T.);
#545=FACE_OUTER_BOUND('',#795,.T.);
#546=FACE_OUTER_BOUND('',#796,.T.);
#547=FACE_OUTER_BOUND('',#797,.T.);
#548=FACE_OUTER_BOUND('',#798,.T.);
#549=FACE_OUTER_BOUND('',#799,.T.);
#550=FACE_OUTER_BOUND('',#800,.T.);
#551=FACE_OUTER_BOUND('',#801,.T.);
#552=FACE_OUTER_BOUND('',#803,.T.);
#553=FACE_OUTER_BOUND('',#804,.T.);
#554=FACE_OUTER_BOUND('',#805,.T.);
#555=FACE_OUTER_BOUND('',#807,.T.);
#556=FACE_OUTER_BOUND('',#808,.T.);
#557=FACE_OUTER_BOUND('',#809,.T.);
#558=FACE_OUTER_BOUND('',#810,.T.);
#559=FACE_OUTER_BOUND('',#811,.T.);
#560=FACE_OUTER_BOUND('',#812,.T.);
#561=FACE_OUTER_BOUND('',#813,.T.);
#562=FACE_OUTER_BOUND('',#814,.T.);
#563=FACE_OUTER_BOUND('',#815,.T.);
#564=FACE_OUTER_BOUND('',#816,.T.);
#565=FACE_OUTER_BOUND('',#817,.T.);
#566=FACE_OUTER_BOUND('',#819,.T.);
#567=FACE_OUTER_BOUND('',#820,.T.);
#568=FACE_OUTER_BOUND('',#821,.T.);
#569=FACE_OUTER_BOUND('',#822,.T.);
#570=FACE_OUTER_BOUND('',#824,.T.);
#571=FACE_OUTER_BOUND('',#827,.T.);
#572=FACE_OUTER_BOUND('',#829,.T.);
#573=FACE_OUTER_BOUND('',#830,.T.);
#574=FACE_OUTER_BOUND('',#832,.T.);
#575=FACE_OUTER_BOUND('',#833,.T.);
#576=FACE_OUTER_BOUND('',#834,.T.);
#577=FACE_OUTER_BOUND('',#835,.T.);
#578=FACE_OUTER_BOUND('',#836,.T.);
#579=FACE_OUTER_BOUND('',#837,.T.);
#580=FACE_OUTER_BOUND('',#838,.T.);
#581=FACE_OUTER_BOUND('',#839,.T.);
#582=FACE_OUTER_BOUND('',#841,.T.);
#583=FACE_OUTER_BOUND('',#842,.T.);
#584=FACE_OUTER_BOUND('',#843,.T.);
#585=FACE_OUTER_BOUND('',#845,.T.);
#586=FACE_OUTER_BOUND('',#846,.T.);
#587=FACE_OUTER_BOUND('',#847,.T.);
#588=FACE_OUTER_BOUND('',#849,.T.);
#589=FACE_OUTER_BOUND('',#851,.T.);
#590=FACE_OUTER_BOUND('',#852,.T.);
#591=FACE_OUTER_BOUND('',#853,.T.);
#592=FACE_OUTER_BOUND('',#855,.T.);
#593=FACE_OUTER_BOUND('',#857,.T.);
#594=FACE_OUTER_BOUND('',#858,.T.);
#595=FACE_OUTER_BOUND('',#859,.T.);
#596=FACE_OUTER_BOUND('',#861,.T.);
#597=FACE_OUTER_BOUND('',#863,.T.);
#598=FACE_OUTER_BOUND('',#864,.T.);
#599=FACE_OUTER_BOUND('',#865,.T.);
#600=FACE_OUTER_BOUND('',#866,.T.);
#601=FACE_OUTER_BOUND('',#867,.T.);
#602=FACE_OUTER_BOUND('',#869,.T.);
#603=FACE_OUTER_BOUND('',#870,.T.);
#604=FACE_OUTER_BOUND('',#871,.T.);
#605=FACE_OUTER_BOUND('',#876,.T.);
#606=FACE_OUTER_BOUND('',#881,.T.);
#607=FACE_OUTER_BOUND('',#882,.T.);
#608=FACE_OUTER_BOUND('',#883,.T.);
#609=FACE_OUTER_BOUND('',#884,.T.);
#610=FACE_OUTER_BOUND('',#885,.T.);
#611=FACE_OUTER_BOUND('',#886,.T.);
#612=FACE_OUTER_BOUND('',#887,.T.);
#613=FACE_OUTER_BOUND('',#888,.T.);
#614=FACE_OUTER_BOUND('',#889,.T.);
#615=FACE_OUTER_BOUND('',#890,.T.);
#616=FACE_OUTER_BOUND('',#893,.T.);
#617=FACE_OUTER_BOUND('',#895,.T.);
#618=FACE_OUTER_BOUND('',#897,.T.);
#619=FACE_OUTER_BOUND('',#899,.T.);
#620=FACE_OUTER_BOUND('',#900,.T.);
#621=FACE_OUTER_BOUND('',#901,.T.);
#622=FACE_OUTER_BOUND('',#902,.T.);
#623=FACE_OUTER_BOUND('',#907,.T.);
#624=FACE_OUTER_BOUND('',#908,.T.);
#625=FACE_OUTER_BOUND('',#909,.T.);
#626=FACE_OUTER_BOUND('',#910,.T.);
#627=FACE_OUTER_BOUND('',#911,.T.);
#628=FACE_OUTER_BOUND('',#913,.T.);
#629=FACE_OUTER_BOUND('',#914,.T.);
#630=FACE_OUTER_BOUND('',#915,.T.);
#631=FACE_OUTER_BOUND('',#916,.T.);
#632=FACE_OUTER_BOUND('',#917,.T.);
#633=FACE_OUTER_BOUND('',#918,.T.);
#634=FACE_OUTER_BOUND('',#919,.T.);
#635=FACE_OUTER_BOUND('',#920,.T.);
#636=FACE_OUTER_BOUND('',#921,.T.);
#637=FACE_OUTER_BOUND('',#922,.T.);
#638=FACE_OUTER_BOUND('',#923,.T.);
#639=FACE_OUTER_BOUND('',#924,.T.);
#640=FACE_OUTER_BOUND('',#925,.T.);
#641=FACE_OUTER_BOUND('',#926,.T.);
#642=FACE_OUTER_BOUND('',#927,.T.);
#643=FACE_OUTER_BOUND('',#928,.T.);
#644=FACE_OUTER_BOUND('',#929,.T.);
#645=FACE_OUTER_BOUND('',#930,.T.);
#646=FACE_OUTER_BOUND('',#932,.T.);
#647=FACE_OUTER_BOUND('',#933,.T.);
#648=FACE_OUTER_BOUND('',#935,.T.);
#649=FACE_OUTER_BOUND('',#936,.T.);
#650=FACE_OUTER_BOUND('',#938,.T.);
#651=FACE_OUTER_BOUND('',#939,.T.);
#652=FACE_OUTER_BOUND('',#941,.T.);
#653=FACE_OUTER_BOUND('',#942,.T.);
#654=FACE_OUTER_BOUND('',#944,.T.);
#655=FACE_OUTER_BOUND('',#945,.T.);
#656=FACE_OUTER_BOUND('',#947,.T.);
#657=FACE_OUTER_BOUND('',#949,.T.);
#658=FACE_OUTER_BOUND('',#950,.T.);
#659=FACE_OUTER_BOUND('',#951,.T.);
#660=FACE_OUTER_BOUND('',#952,.T.);
#661=FACE_OUTER_BOUND('',#953,.T.);
#662=FACE_OUTER_BOUND('',#955,.T.);
#663=FACE_OUTER_BOUND('',#957,.T.);
#664=FACE_OUTER_BOUND('',#959,.T.);
#665=FACE_OUTER_BOUND('',#961,.T.);
#666=FACE_OUTER_BOUND('',#962,.T.);
#667=FACE_OUTER_BOUND('',#963,.T.);
#668=FACE_OUTER_BOUND('',#964,.T.);
#669=FACE_OUTER_BOUND('',#965,.T.);
#670=FACE_OUTER_BOUND('',#966,.T.);
#671=FACE_OUTER_BOUND('',#968,.T.);
#672=FACE_OUTER_BOUND('',#970,.T.);
#673=FACE_OUTER_BOUND('',#971,.T.);
#674=FACE_OUTER_BOUND('',#972,.T.);
#675=FACE_OUTER_BOUND('',#973,.T.);
#676=FACE_OUTER_BOUND('',#974,.T.);
#677=FACE_OUTER_BOUND('',#975,.T.);
#678=FACE_OUTER_BOUND('',#977,.T.);
#679=FACE_OUTER_BOUND('',#979,.T.);
#680=FACE_OUTER_BOUND('',#980,.T.);
#681=FACE_OUTER_BOUND('',#982,.T.);
#682=FACE_OUTER_BOUND('',#983,.T.);
#683=FACE_OUTER_BOUND('',#984,.T.);
#684=FACE_OUTER_BOUND('',#986,.T.);
#685=FACE_OUTER_BOUND('',#988,.T.);
#686=FACE_OUTER_BOUND('',#989,.T.);
#687=FACE_OUTER_BOUND('',#990,.T.);
#688=FACE_OUTER_BOUND('',#991,.T.);
#689=FACE_OUTER_BOUND('',#992,.T.);
#690=FACE_OUTER_BOUND('',#993,.T.);
#691=FACE_OUTER_BOUND('',#994,.T.);
#692=FACE_OUTER_BOUND('',#996,.T.);
#693=FACE_OUTER_BOUND('',#997,.T.);
#694=FACE_OUTER_BOUND('',#998,.T.);
#695=FACE_OUTER_BOUND('',#999,.T.);
#696=FACE_OUTER_BOUND('',#1000,.T.);
#697=FACE_OUTER_BOUND('',#1001,.T.);
#698=FACE_OUTER_BOUND('',#1002,.T.);
#699=FACE_OUTER_BOUND('',#1003,.T.);
#700=FACE_OUTER_BOUND('',#1005,.T.);
#701=FACE_OUTER_BOUND('',#1006,.T.);
#702=FACE_OUTER_BOUND('',#1007,.T.);
#703=FACE_OUTER_BOUND('',#1008,.T.);
#704=FACE_OUTER_BOUND('',#1009,.T.);
#705=FACE_OUTER_BOUND('',#1010,.T.);
#706=FACE_OUTER_BOUND('',#1011,.T.);
#707=FACE_OUTER_BOUND('',#1012,.T.);
#708=FACE_OUTER_BOUND('',#1013,.T.);
#709=FACE_OUTER_BOUND('',#1015,.T.);
#710=FACE_OUTER_BOUND('',#1016,.T.);
#711=FACE_OUTER_BOUND('',#1017,.T.);
#712=FACE_OUTER_BOUND('',#1018,.T.);
#713=FACE_OUTER_BOUND('',#1019,.T.);
#714=FACE_OUTER_BOUND('',#1020,.T.);
#715=FACE_OUTER_BOUND('',#1021,.T.);
#716=FACE_OUTER_BOUND('',#1022,.T.);
#717=FACE_OUTER_BOUND('',#1023,.T.);
#718=FACE_OUTER_BOUND('',#1024,.T.);
#719=FACE_OUTER_BOUND('',#1025,.T.);
#720=FACE_OUTER_BOUND('',#1026,.T.);
#721=EDGE_LOOP('',(#2642,#2643,#2644,#2645));
#722=EDGE_LOOP('',(#2646,#2647,#2648,#2649));
#723=EDGE_LOOP('',(#2650,#2651,#2652,#2653));
#724=EDGE_LOOP('',(#2654,#2655,#2656,#2657));
#725=EDGE_LOOP('',(#2658,#2659,#2660,#2661));
#726=EDGE_LOOP('',(#2662,#2663,#2664,#2665));
#727=EDGE_LOOP('',(#2666,#2667,#2668,#2669));
#728=EDGE_LOOP('',(#2670,#2671,#2672,#2673));
#729=EDGE_LOOP('',(#2674,#2675,#2676,#2677));
#730=EDGE_LOOP('',(#2678));
#731=EDGE_LOOP('',(#2679));
#732=EDGE_LOOP('',(#2680));
#733=EDGE_LOOP('',(#2681));
#734=EDGE_LOOP('',(#2682,#2683,#2684,#2685));
#735=EDGE_LOOP('',(#2686));
#736=EDGE_LOOP('',(#2687));
#737=EDGE_LOOP('',(#2688));
#738=EDGE_LOOP('',(#2689));
#739=EDGE_LOOP('',(#2690,#2691,#2692,#2693,#2694,#2695,#2696,#2697));
#740=EDGE_LOOP('',(#2698,#2699,#2700));
#741=EDGE_LOOP('',(#2701,#2702,#2703,#2704,#2705,#2706,#2707,#2708));
#742=EDGE_LOOP('',(#2709,#2710));
#743=EDGE_LOOP('',(#2711,#2712,#2713,#2714,#2715,#2716,#2717,#2718));
#744=EDGE_LOOP('',(#2719,#2720));
#745=EDGE_LOOP('',(#2721));
#746=EDGE_LOOP('',(#2722,#2723,#2724,#2725,#2726,#2727,#2728,#2729,#2730));
#747=EDGE_LOOP('',(#2731,#2732,#2733));
#748=EDGE_LOOP('',(#2734,#2735,#2736,#2737,#2738,#2739,#2740,#2741));
#749=EDGE_LOOP('',(#2742,#2743));
#750=EDGE_LOOP('',(#2744,#2745,#2746,#2747,#2748,#2749,#2750,#2751));
#751=EDGE_LOOP('',(#2752,#2753));
#752=EDGE_LOOP('',(#2754,#2755,#2756,#2757,#2758,#2759,#2760,#2761));
#753=EDGE_LOOP('',(#2762,#2763,#2764,#2765,#2766,#2767,#2768,#2769,#2770,
#2771,#2772,#2773,#2774,#2775,#2776,#2777,#2778,#2779,#2780,#2781,#2782,
#2783,#2784,#2785,#2786,#2787,#2788,#2789));
#754=EDGE_LOOP('',(#2790,#2791,#2792,#2793));
#755=EDGE_LOOP('',(#2794));
#756=EDGE_LOOP('',(#2795,#2796,#2797,#2798,#2799,#2800,#2801,#2802,#2803));
#757=EDGE_LOOP('',(#2804,#2805,#2806,#2807));
#758=EDGE_LOOP('',(#2808,#2809,#2810,#2811));
#759=EDGE_LOOP('',(#2812));
#760=EDGE_LOOP('',(#2813));
#761=EDGE_LOOP('',(#2814));
#762=EDGE_LOOP('',(#2815));
#763=EDGE_LOOP('',(#2816));
#764=EDGE_LOOP('',(#2817));
#765=EDGE_LOOP('',(#2818));
#766=EDGE_LOOP('',(#2819));
#767=EDGE_LOOP('',(#2820));
#768=EDGE_LOOP('',(#2821));
#769=EDGE_LOOP('',(#2822,#2823,#2824,#2825));
#770=EDGE_LOOP('',(#2826));
#771=EDGE_LOOP('',(#2827,#2828,#2829,#2830));
#772=EDGE_LOOP('',(#2831));
#773=EDGE_LOOP('',(#2832,#2833,#2834,#2835));
#774=EDGE_LOOP('',(#2836));
#775=EDGE_LOOP('',(#2837,#2838,#2839,#2840));
#776=EDGE_LOOP('',(#2841));
#777=EDGE_LOOP('',(#2842,#2843,#2844,#2845));
#778=EDGE_LOOP('',(#2846,#2847,#2848,#2849,#2850,#2851));
#779=EDGE_LOOP('',(#2852,#2853,#2854,#2855));
#780=EDGE_LOOP('',(#2856));
#781=EDGE_LOOP('',(#2857,#2858,#2859,#2860));
#782=EDGE_LOOP('',(#2861,#2862,#2863,#2864));
#783=EDGE_LOOP('',(#2865,#2866,#2867,#2868,#2869,#2870));
#784=EDGE_LOOP('',(#2871,#2872,#2873,#2874));
#785=EDGE_LOOP('',(#2875));
#786=EDGE_LOOP('',(#2876,#2877,#2878,#2879));
#787=EDGE_LOOP('',(#2880));
#788=EDGE_LOOP('',(#2881));
#789=EDGE_LOOP('',(#2882,#2883));
#790=EDGE_LOOP('',(#2884));
#791=EDGE_LOOP('',(#2885,#2886,#2887,#2888));
#792=EDGE_LOOP('',(#2889,#2890));
#793=EDGE_LOOP('',(#2891));
#794=EDGE_LOOP('',(#2892,#2893,#2894,#2895));
#795=EDGE_LOOP('',(#2896,#2897,#2898,#2899,#2900,#2901,#2902,#2903));
#796=EDGE_LOOP('',(#2904,#2905,#2906,#2907,#2908,#2909,#2910,#2911));
#797=EDGE_LOOP('',(#2912,#2913,#2914,#2915));
#798=EDGE_LOOP('',(#2916,#2917,#2918,#2919));
#799=EDGE_LOOP('',(#2920,#2921,#2922,#2923));
#800=EDGE_LOOP('',(#2924,#2925,#2926,#2927,#2928,#2929));
#801=EDGE_LOOP('',(#2930,#2931,#2932,#2933));
#802=EDGE_LOOP('',(#2934));
#803=EDGE_LOOP('',(#2935,#2936,#2937,#2938,#2939,#2940));
#804=EDGE_LOOP('',(#2941,#2942,#2943,#2944,#2945,#2946,#2947,#2948));
#805=EDGE_LOOP('',(#2949,#2950,#2951,#2952));
#806=EDGE_LOOP('',(#2953));
#807=EDGE_LOOP('',(#2954,#2955,#2956,#2957));
#808=EDGE_LOOP('',(#2958));
#809=EDGE_LOOP('',(#2959,#2960,#2961,#2962));
#810=EDGE_LOOP('',(#2963));
#811=EDGE_LOOP('',(#2964,#2965,#2966,#2967));
#812=EDGE_LOOP('',(#2968));
#813=EDGE_LOOP('',(#2969,#2970,#2971,#2972));
#814=EDGE_LOOP('',(#2973));
#815=EDGE_LOOP('',(#2974,#2975,#2976,#2977));
#816=EDGE_LOOP('',(#2978,#2979,#2980,#2981,#2982,#2983));
#817=EDGE_LOOP('',(#2984,#2985,#2986,#2987));
#818=EDGE_LOOP('',(#2988));
#819=EDGE_LOOP('',(#2989,#2990,#2991,#2992));
#820=EDGE_LOOP('',(#2993,#2994,#2995,#2996));
#821=EDGE_LOOP('',(#2997,#2998,#2999,#3000,#3001,#3002));
#822=EDGE_LOOP('',(#3003,#3004,#3005,#3006));
#823=EDGE_LOOP('',(#3007));
#824=EDGE_LOOP('',(#3008,#3009,#3010,#3011));
#825=EDGE_LOOP('',(#3012));
#826=EDGE_LOOP('',(#3013));
#827=EDGE_LOOP('',(#3014,#3015));
#828=EDGE_LOOP('',(#3016));
#829=EDGE_LOOP('',(#3017,#3018,#3019,#3020));
#830=EDGE_LOOP('',(#3021,#3022));
#831=EDGE_LOOP('',(#3023));
#832=EDGE_LOOP('',(#3024,#3025,#3026,#3027));
#833=EDGE_LOOP('',(#3028,#3029,#3030,#3031,#3032,#3033,#3034,#3035));
#834=EDGE_LOOP('',(#3036,#3037,#3038,#3039,#3040,#3041,#3042,#3043));
#835=EDGE_LOOP('',(#3044,#3045,#3046,#3047));
#836=EDGE_LOOP('',(#3048,#3049,#3050,#3051));
#837=EDGE_LOOP('',(#3052,#3053,#3054,#3055));
#838=EDGE_LOOP('',(#3056,#3057,#3058,#3059,#3060,#3061));
#839=EDGE_LOOP('',(#3062,#3063,#3064,#3065));
#840=EDGE_LOOP('',(#3066));
#841=EDGE_LOOP('',(#3067,#3068,#3069,#3070,#3071,#3072));
#842=EDGE_LOOP('',(#3073,#3074,#3075,#3076,#3077,#3078,#3079,#3080));
#843=EDGE_LOOP('',(#3081,#3082,#3083,#3084));
#844=EDGE_LOOP('',(#3085));
#845=EDGE_LOOP('',(#3086,#3087,#3088,#3089));
#846=EDGE_LOOP('',(#3090,#3091,#3092,#3093));
#847=EDGE_LOOP('',(#3094));
#848=EDGE_LOOP('',(#3095));
#849=EDGE_LOOP('',(#3096));
#850=EDGE_LOOP('',(#3097));
#851=EDGE_LOOP('',(#3098,#3099,#3100,#3101));
#852=EDGE_LOOP('',(#3102,#3103,#3104,#3105));
#853=EDGE_LOOP('',(#3106));
#854=EDGE_LOOP('',(#3107));
#855=EDGE_LOOP('',(#3108));
#856=EDGE_LOOP('',(#3109));
#857=EDGE_LOOP('',(#3110,#3111,#3112,#3113));
#858=EDGE_LOOP('',(#3114,#3115,#3116,#3117));
#859=EDGE_LOOP('',(#3118));
#860=EDGE_LOOP('',(#3119));
#861=EDGE_LOOP('',(#3120));
#862=EDGE_LOOP('',(#3121));
#863=EDGE_LOOP('',(#3122,#3123,#3124,#3125));
#864=EDGE_LOOP('',(#3126,#3127,#3128,#3129));
#865=EDGE_LOOP('',(#3130,#3131,#3132,#3133));
#866=EDGE_LOOP('',(#3134,#3135,#3136,#3137));
#867=EDGE_LOOP('',(#3138));
#868=EDGE_LOOP('',(#3139));
#869=EDGE_LOOP('',(#3140,#3141,#3142,#3143));
#870=EDGE_LOOP('',(#3144,#3145,#3146,#3147));
#871=EDGE_LOOP('',(#3148));
#872=EDGE_LOOP('',(#3149));
#873=EDGE_LOOP('',(#3150));
#874=EDGE_LOOP('',(#3151));
#875=EDGE_LOOP('',(#3152));
#876=EDGE_LOOP('',(#3153));
#877=EDGE_LOOP('',(#3154));
#878=EDGE_LOOP('',(#3155));
#879=EDGE_LOOP('',(#3156));
#880=EDGE_LOOP('',(#3157));
#881=EDGE_LOOP('',(#3158,#3159));
#882=EDGE_LOOP('',(#3160,#3161,#3162,#3163,#3164,#3165));
#883=EDGE_LOOP('',(#3166,#3167,#3168,#3169,#3170));
#884=EDGE_LOOP('',(#3171,#3172));
#885=EDGE_LOOP('',(#3173,#3174,#3175,#3176,#3177,#3178,#3179,#3180));
#886=EDGE_LOOP('',(#3181,#3182));
#887=EDGE_LOOP('',(#3183,#3184,#3185,#3186,#3187,#3188,#3189,#3190));
#888=EDGE_LOOP('',(#3191,#3192));
#889=EDGE_LOOP('',(#3193,#3194,#3195,#3196,#3197,#3198,#3199,#3200));
#890=EDGE_LOOP('',(#3201,#3202,#3203,#3204,#3205,#3206,#3207,#3208,#3209,
#3210,#3211,#3212,#3213,#3214,#3215,#3216));
#891=EDGE_LOOP('',(#3217,#3218,#3219));
#892=EDGE_LOOP('',(#3220,#3221));
#893=EDGE_LOOP('',(#3222,#3223,#3224,#3225));
#894=EDGE_LOOP('',(#3226));
#895=EDGE_LOOP('',(#3227,#3228,#3229,#3230));
#896=EDGE_LOOP('',(#3231));
#897=EDGE_LOOP('',(#3232));
#898=EDGE_LOOP('',(#3233,#3234,#3235,#3236,#3237,#3238,#3239,#3240,#3241,
#3242,#3243,#3244,#3245));
#899=EDGE_LOOP('',(#3246,#3247,#3248,#3249,#3250));
#900=EDGE_LOOP('',(#3251,#3252,#3253,#3254,#3255,#3256,#3257,#3258));
#901=EDGE_LOOP('',(#3259,#3260,#3261,#3262));
#902=EDGE_LOOP('',(#3263));
#903=EDGE_LOOP('',(#3264));
#904=EDGE_LOOP('',(#3265));
#905=EDGE_LOOP('',(#3266));
#906=EDGE_LOOP('',(#3267));
#907=EDGE_LOOP('',(#3268));
#908=EDGE_LOOP('',(#3269,#3270,#3271,#3272));
#909=EDGE_LOOP('',(#3273,#3274,#3275,#3276));
#910=EDGE_LOOP('',(#3277,#3278,#3279,#3280));
#911=EDGE_LOOP('',(#3281));
#912=EDGE_LOOP('',(#3282));
#913=EDGE_LOOP('',(#3283,#3284,#3285,#3286));
#914=EDGE_LOOP('',(#3287,#3288,#3289,#3290));
#915=EDGE_LOOP('',(#3291,#3292,#3293,#3294));
#916=EDGE_LOOP('',(#3295));
#917=EDGE_LOOP('',(#3296,#3297,#3298,#3299));
#918=EDGE_LOOP('',(#3300,#3301,#3302,#3303));
#919=EDGE_LOOP('',(#3304,#3305,#3306,#3307));
#920=EDGE_LOOP('',(#3308,#3309,#3310,#3311));
#921=EDGE_LOOP('',(#3312,#3313,#3314,#3315));
#922=EDGE_LOOP('',(#3316,#3317,#3318,#3319));
#923=EDGE_LOOP('',(#3320,#3321,#3322,#3323,#3324,#3325));
#924=EDGE_LOOP('',(#3326,#3327,#3328,#3329,#3330,#3331));
#925=EDGE_LOOP('',(#3332,#3333,#3334,#3335));
#926=EDGE_LOOP('',(#3336,#3337,#3338,#3339));
#927=EDGE_LOOP('',(#3340,#3341,#3342,#3343));
#928=EDGE_LOOP('',(#3344,#3345,#3346,#3347));
#929=EDGE_LOOP('',(#3348,#3349,#3350,#3351));
#930=EDGE_LOOP('',(#3352));
#931=EDGE_LOOP('',(#3353));
#932=EDGE_LOOP('',(#3354,#3355,#3356,#3357));
#933=EDGE_LOOP('',(#3358));
#934=EDGE_LOOP('',(#3359));
#935=EDGE_LOOP('',(#3360,#3361,#3362,#3363));
#936=EDGE_LOOP('',(#3364));
#937=EDGE_LOOP('',(#3365));
#938=EDGE_LOOP('',(#3366,#3367,#3368,#3369));
#939=EDGE_LOOP('',(#3370));
#940=EDGE_LOOP('',(#3371));
#941=EDGE_LOOP('',(#3372,#3373,#3374,#3375));
#942=EDGE_LOOP('',(#3376));
#943=EDGE_LOOP('',(#3377));
#944=EDGE_LOOP('',(#3378,#3379,#3380,#3381));
#945=EDGE_LOOP('',(#3382));
#946=EDGE_LOOP('',(#3383));
#947=EDGE_LOOP('',(#3384,#3385,#3386,#3387));
#948=EDGE_LOOP('',(#3388,#3389,#3390,#3391));
#949=EDGE_LOOP('',(#3392,#3393,#3394,#3395));
#950=EDGE_LOOP('',(#3396,#3397,#3398,#3399));
#951=EDGE_LOOP('',(#3400,#3401,#3402,#3403));
#952=EDGE_LOOP('',(#3404,#3405,#3406,#3407));
#953=EDGE_LOOP('',(#3408));
#954=EDGE_LOOP('',(#3409));
#955=EDGE_LOOP('',(#3410,#3411,#3412,#3413));
#956=EDGE_LOOP('',(#3414,#3415,#3416,#3417));
#957=EDGE_LOOP('',(#3418));
#958=EDGE_LOOP('',(#3419));
#959=EDGE_LOOP('',(#3420,#3421,#3422,#3423));
#960=EDGE_LOOP('',(#3424,#3425,#3426,#3427));
#961=EDGE_LOOP('',(#3428,#3429));
#962=EDGE_LOOP('',(#3430,#3431,#3432,#3433,#3434,#3435,#3436,#3437,#3438,
#3439,#3440));
#963=EDGE_LOOP('',(#3441,#3442));
#964=EDGE_LOOP('',(#3443,#3444,#3445,#3446,#3447,#3448,#3449,#3450,#3451,
#3452,#3453,#3454));
#965=EDGE_LOOP('',(#3455,#3456,#3457,#3458,#3459,#3460,#3461,#3462,#3463));
#966=EDGE_LOOP('',(#3464));
#967=EDGE_LOOP('',(#3465));
#968=EDGE_LOOP('',(#3466));
#969=EDGE_LOOP('',(#3467));
#970=EDGE_LOOP('',(#3468,#3469));
#971=EDGE_LOOP('',(#3470,#3471,#3472,#3473,#3474,#3475,#3476,#3477,#3478,
#3479,#3480));
#972=EDGE_LOOP('',(#3481,#3482));
#973=EDGE_LOOP('',(#3483,#3484,#3485,#3486,#3487,#3488,#3489,#3490,#3491,
#3492,#3493,#3494));
#974=EDGE_LOOP('',(#3495,#3496,#3497,#3498,#3499,#3500,#3501,#3502,#3503));
#975=EDGE_LOOP('',(#3504));
#976=EDGE_LOOP('',(#3505));
#977=EDGE_LOOP('',(#3506));
#978=EDGE_LOOP('',(#3507));
#979=EDGE_LOOP('',(#3508,#3509,#3510,#3511));
#980=EDGE_LOOP('',(#3512));
#981=EDGE_LOOP('',(#3513));
#982=EDGE_LOOP('',(#3514,#3515,#3516,#3517));
#983=EDGE_LOOP('',(#3518,#3519,#3520,#3521));
#984=EDGE_LOOP('',(#3522));
#985=EDGE_LOOP('',(#3523));
#986=EDGE_LOOP('',(#3524));
#987=EDGE_LOOP('',(#3525));
#988=EDGE_LOOP('',(#3526,#3527,#3528,#3529));
#989=EDGE_LOOP('',(#3530));
#990=EDGE_LOOP('',(#3531,#3532,#3533,#3534));
#991=EDGE_LOOP('',(#3535,#3536,#3537,#3538));
#992=EDGE_LOOP('',(#3539));
#993=EDGE_LOOP('',(#3540,#3541,#3542,#3543));
#994=EDGE_LOOP('',(#3544));
#995=EDGE_LOOP('',(#3545));
#996=EDGE_LOOP('',(#3546,#3547,#3548,#3549));
#997=EDGE_LOOP('',(#3550,#3551,#3552,#3553));
#998=EDGE_LOOP('',(#3554,#3555,#3556,#3557));
#999=EDGE_LOOP('',(#3558,#3559,#3560,#3561));
#1000=EDGE_LOOP('',(#3562,#3563,#3564,#3565));
#1001=EDGE_LOOP('',(#3566,#3567,#3568,#3569));
#1002=EDGE_LOOP('',(#3570,#3571,#3572,#3573,#3574,#3575));
#1003=EDGE_LOOP('',(#3576));
#1004=EDGE_LOOP('',(#3577,#3578,#3579,#3580,#3581,#3582));
#1005=EDGE_LOOP('',(#3583,#3584,#3585,#3586));
#1006=EDGE_LOOP('',(#3587,#3588,#3589,#3590));
#1007=EDGE_LOOP('',(#3591,#3592,#3593,#3594));
#1008=EDGE_LOOP('',(#3595));
#1009=EDGE_LOOP('',(#3596));
#1010=EDGE_LOOP('',(#3597,#3598,#3599,#3600));
#1011=EDGE_LOOP('',(#3601,#3602,#3603,#3604));
#1012=EDGE_LOOP('',(#3605,#3606,#3607,#3608));
#1013=EDGE_LOOP('',(#3609));
#1014=EDGE_LOOP('',(#3610));
#1015=EDGE_LOOP('',(#3611,#3612,#3613,#3614));
#1016=EDGE_LOOP('',(#3615,#3616,#3617,#3618));
#1017=EDGE_LOOP('',(#3619,#3620,#3621,#3622));
#1018=EDGE_LOOP('',(#3623));
#1019=EDGE_LOOP('',(#3624,#3625,#3626,#3627));
#1020=EDGE_LOOP('',(#3628,#3629,#3630,#3631));
#1021=EDGE_LOOP('',(#3632,#3633,#3634,#3635));
#1022=EDGE_LOOP('',(#3636,#3637,#3638,#3639));
#1023=EDGE_LOOP('',(#3640,#3641,#3642,#3643));
#1024=EDGE_LOOP('',(#3644,#3645,#3646,#3647));
#1025=EDGE_LOOP('',(#3648,#3649,#3650,#3651,#3652,#3653));
#1026=EDGE_LOOP('',(#3654,#3655,#3656,#3657,#3658,#3659));
#1027=LINE('',#5994,#1307);
#1028=LINE('',#6000,#1308);
#1029=LINE('',#6006,#1309);
#1030=LINE('',#6012,#1310);
#1031=LINE('',#6017,#1311);
#1032=LINE('',#6019,#1312);
#1033=LINE('',#6021,#1313);
#1034=LINE('',#6022,#1314);
#1035=LINE('',#6025,#1315);
#1036=LINE('',#6027,#1316);
#1037=LINE('',#6028,#1317);
#1038=LINE('',#6031,#1318);
#1039=LINE('',#6033,#1319);
#1040=LINE('',#6034,#1320);
#1041=LINE('',#6036,#1321);
#1042=LINE('',#6037,#1322);
#1043=LINE('',#6044,#1323);
#1044=LINE('',#6048,#1324);
#1045=LINE('',#6052,#1325);
#1046=LINE('',#6062,#1326);
#1047=LINE('',#6066,#1327);
#1048=LINE('',#6070,#1328);
#1049=LINE('',#6078,#1329);
#1050=LINE('',#6082,#1330);
#1051=LINE('',#6086,#1331);
#1052=LINE('',#6108,#1332);
#1053=LINE('',#6111,#1333);
#1054=LINE('',#6113,#1334);
#1055=LINE('',#6124,#1335);
#1056=LINE('',#6127,#1336);
#1057=LINE('',#6129,#1337);
#1058=LINE('',#6140,#1338);
#1059=LINE('',#6143,#1339);
#1060=LINE('',#6145,#1340);
#1061=LINE('',#6148,#1341);
#1062=LINE('',#6155,#1342);
#1063=LINE('',#6161,#1343);
#1064=LINE('',#6167,#1344);
#1065=LINE('',#6176,#1345);
#1066=LINE('',#6183,#1346);
#1067=LINE('',#6190,#1347);
#1068=LINE('',#6197,#1348);
#1069=LINE('',#6205,#1349);
#1070=LINE('',#6208,#1350);
#1071=LINE('',#6211,#1351);
#1072=LINE('',#6213,#1352);
#1073=LINE('',#6215,#1353);
#1074=LINE('',#6217,#1354);
#1075=LINE('',#6218,#1355);
#1076=LINE('',#6221,#1356);
#1077=LINE('',#6222,#1357);
#1078=LINE('',#6225,#1358);
#1079=LINE('',#6227,#1359);
#1080=LINE('',#6228,#1360);
#1081=LINE('',#6231,#1361);
#1082=LINE('',#6232,#1362);
#1083=LINE('',#6234,#1363);
#1084=LINE('',#6235,#1364);
#1085=LINE('',#6242,#1365);
#1086=LINE('',#6248,#1366);
#1087=LINE('',#6251,#1367);
#1088=LINE('',#6255,#1368);
#1089=LINE('',#6261,#1369);
#1090=LINE('',#6264,#1370);
#1091=LINE('',#6267,#1371);
#1092=LINE('',#6269,#1372);
#1093=LINE('',#6271,#1373);
#1094=LINE('',#6273,#1374);
#1095=LINE('',#6274,#1375);
#1096=LINE('',#6277,#1376);
#1097=LINE('',#6279,#1377);
#1098=LINE('',#6281,#1378);
#1099=LINE('',#6283,#1379);
#1100=LINE('',#6284,#1380);
#1101=LINE('',#6288,#1381);
#1102=LINE('',#6292,#1382);
#1103=LINE('',#6298,#1383);
#1104=LINE('',#6301,#1384);
#1105=LINE('',#6303,#1385);
#1106=LINE('',#6304,#1386);
#1107=LINE('',#6305,#1387);
#1108=LINE('',#6307,#1388);
#1109=LINE('',#6309,#1389);
#1110=LINE('',#6310,#1390);
#1111=LINE('',#6318,#1391);
#1112=LINE('',#6325,#1392);
#1113=LINE('',#6332,#1393);
#1114=LINE('',#6339,#1394);
#1115=LINE('',#6347,#1395);
#1116=LINE('',#6350,#1396);
#1117=LINE('',#6353,#1397);
#1118=LINE('',#6355,#1398);
#1119=LINE('',#6357,#1399);
#1120=LINE('',#6359,#1400);
#1121=LINE('',#6360,#1401);
#1122=LINE('',#6363,#1402);
#1123=LINE('',#6364,#1403);
#1124=LINE('',#6367,#1404);
#1125=LINE('',#6369,#1405);
#1126=LINE('',#6370,#1406);
#1127=LINE('',#6373,#1407);
#1128=LINE('',#6374,#1408);
#1129=LINE('',#6376,#1409);
#1130=LINE('',#6377,#1410);
#1131=LINE('',#6384,#1411);
#1132=LINE('',#6390,#1412);
#1133=LINE('',#6393,#1413);
#1134=LINE('',#6397,#1414);
#1135=LINE('',#6403,#1415);
#1136=LINE('',#6406,#1416);
#1137=LINE('',#6409,#1417);
#1138=LINE('',#6411,#1418);
#1139=LINE('',#6413,#1419);
#1140=LINE('',#6415,#1420);
#1141=LINE('',#6416,#1421);
#1142=LINE('',#6419,#1422);
#1143=LINE('',#6421,#1423);
#1144=LINE('',#6423,#1424);
#1145=LINE('',#6425,#1425);
#1146=LINE('',#6426,#1426);
#1147=LINE('',#6430,#1427);
#1148=LINE('',#6434,#1428);
#1149=LINE('',#6440,#1429);
#1150=LINE('',#6443,#1430);
#1151=LINE('',#6445,#1431);
#1152=LINE('',#6446,#1432);
#1153=LINE('',#6447,#1433);
#1154=LINE('',#6449,#1434);
#1155=LINE('',#6451,#1435);
#1156=LINE('',#6452,#1436);
#1157=LINE('',#6460,#1437);
#1158=LINE('',#6466,#1438);
#1159=LINE('',#6475,#1439);
#1160=LINE('',#6481,#1440);
#1161=LINE('',#6490,#1441);
#1162=LINE('',#6496,#1442);
#1163=LINE('',#6505,#1443);
#1164=LINE('',#6511,#1444);
#1165=LINE('',#6517,#1445);
#1166=LINE('',#6523,#1446);
#1167=LINE('',#6531,#1447);
#1168=LINE('',#6536,#1448);
#1169=LINE('',#6544,#1449);
#1170=LINE('',#6550,#1450);
#1171=LINE('',#6629,#1451);
#1172=LINE('',#6640,#1452);
#1173=LINE('',#6643,#1453);
#1174=LINE('',#6645,#1454);
#1175=LINE('',#6656,#1455);
#1176=LINE('',#6659,#1456);
#1177=LINE('',#6661,#1457);
#1178=LINE('',#6672,#1458);
#1179=LINE('',#6675,#1459);
#1180=LINE('',#6677,#1460);
#1181=LINE('',#6685,#1461);
#1182=LINE('',#6689,#1462);
#1183=LINE('',#6694,#1463);
#1184=LINE('',#6695,#1464);
#1185=LINE('',#6696,#1465);
#1186=LINE('',#6700,#1466);
#1187=LINE('',#6701,#1467);
#1188=LINE('',#6702,#1468);
#1189=LINE('',#6713,#1469);
#1190=LINE('',#6717,#1470);
#1191=LINE('',#6727,#1471);
#1192=LINE('',#6731,#1472);
#1193=LINE('',#6735,#1473);
#1194=LINE('',#6742,#1474);
#1195=LINE('',#6746,#1475);
#1196=LINE('',#6750,#1476);
#1197=LINE('',#6755,#1477);
#1198=LINE('',#6757,#1478);
#1199=LINE('',#6759,#1479);
#1200=LINE('',#6760,#1480);
#1201=LINE('',#6763,#1481);
#1202=LINE('',#6765,#1482);
#1203=LINE('',#6766,#1483);
#1204=LINE('',#6769,#1484);
#1205=LINE('',#6771,#1485);
#1206=LINE('',#6772,#1486);
#1207=LINE('',#6775,#1487);
#1208=LINE('',#6777,#1488);
#1209=LINE('',#6778,#1489);
#1210=LINE('',#6781,#1490);
#1211=LINE('',#6783,#1491);
#1212=LINE('',#6784,#1492);
#1213=LINE('',#6786,#1493);
#1214=LINE('',#6787,#1494);
#1215=LINE('',#6797,#1495);
#1216=LINE('',#6799,#1496);
#1217=LINE('',#6800,#1497);
#1218=LINE('',#6803,#1498);
#1219=LINE('',#6805,#1499);
#1220=LINE('',#6806,#1500);
#1221=LINE('',#6811,#1501);
#1222=LINE('',#6812,#1502);
#1223=LINE('',#6814,#1503);
#1224=LINE('',#6815,#1504);
#1225=LINE('',#6825,#1505);
#1226=LINE('',#6832,#1506);
#1227=LINE('',#6839,#1507);
#1228=LINE('',#6846,#1508);
#1229=LINE('',#6853,#1509);
#1230=LINE('',#6858,#1510);
#1231=LINE('',#6865,#1511);
#1232=LINE('',#6868,#1512);
#1233=LINE('',#6871,#1513);
#1234=LINE('',#6873,#1514);
#1235=LINE('',#6874,#1515);
#1236=LINE('',#6880,#1516);
#1237=LINE('',#6882,#1517);
#1238=LINE('',#6883,#1518);
#1239=LINE('',#6892,#1519);
#1240=LINE('',#6897,#1520);
#1241=LINE('',#6905,#1521);
#1242=LINE('',#6938,#1522);
#1243=LINE('',#6980,#1523);
#1244=LINE('',#6984,#1524);
#1245=LINE('',#6986,#1525);
#1246=LINE('',#6991,#1526);
#1247=LINE('',#6993,#1527);
#1248=LINE('',#7001,#1528);
#1249=LINE('',#7034,#1529);
#1250=LINE('',#7076,#1530);
#1251=LINE('',#7080,#1531);
#1252=LINE('',#7082,#1532);
#1253=LINE('',#7087,#1533);
#1254=LINE('',#7089,#1534);
#1255=LINE('',#7098,#1535);
#1256=LINE('',#7105,#1536);
#1257=LINE('',#7111,#1537);
#1258=LINE('',#7120,#1538);
#1259=LINE('',#7127,#1539);
#1260=LINE('',#7132,#1540);
#1261=LINE('',#7137,#1541);
#1262=LINE('',#7143,#1542);
#1263=LINE('',#7145,#1543);
#1264=LINE('',#7147,#1544);
#1265=LINE('',#7148,#1545);
#1266=LINE('',#7151,#1546);
#1267=LINE('',#7153,#1547);
#1268=LINE('',#7154,#1548);
#1269=LINE('',#7157,#1549);
#1270=LINE('',#7159,#1550);
#1271=LINE('',#7160,#1551);
#1272=LINE('',#7163,#1552);
#1273=LINE('',#7165,#1553);
#1274=LINE('',#7166,#1554);
#1275=LINE('',#7169,#1555);
#1276=LINE('',#7171,#1556);
#1277=LINE('',#7172,#1557);
#1278=LINE('',#7174,#1558);
#1279=LINE('',#7175,#1559);
#1280=LINE('',#7183,#1560);
#1281=LINE('',#7187,#1561);
#1282=LINE('',#7191,#1562);
#1283=LINE('',#7200,#1563);
#1284=LINE('',#7204,#1564);
#1285=LINE('',#7208,#1565);
#1286=LINE('',#7215,#1566);
#1287=LINE('',#7219,#1567);
#1288=LINE('',#7223,#1568);
#1289=LINE('',#7228,#1569);
#1290=LINE('',#7230,#1570);
#1291=LINE('',#7232,#1571);
#1292=LINE('',#7233,#1572);
#1293=LINE('',#7236,#1573);
#1294=LINE('',#7238,#1574);
#1295=LINE('',#7239,#1575);
#1296=LINE('',#7242,#1576);
#1297=LINE('',#7244,#1577);
#1298=LINE('',#7245,#1578);
#1299=LINE('',#7248,#1579);
#1300=LINE('',#7250,#1580);
#1301=LINE('',#7251,#1581);
#1302=LINE('',#7254,#1582);
#1303=LINE('',#7256,#1583);
#1304=LINE('',#7257,#1584);
#1305=LINE('',#7259,#1585);
#1306=LINE('',#7260,#1586);
#1307=VECTOR('',#4717,0.274999999999999);
#1308=VECTOR('',#4724,0.275);
#1309=VECTOR('',#4731,0.275);
#1310=VECTOR('',#4738,0.274999999999999);
#1311=VECTOR('',#4743,1.);
#1312=VECTOR('',#4744,1.);
#1313=VECTOR('',#4745,1.);
#1314=VECTOR('',#4746,1.);
#1315=VECTOR('',#4749,1.);
#1316=VECTOR('',#4750,1.);
#1317=VECTOR('',#4751,1.);
#1318=VECTOR('',#4754,1.);
#1319=VECTOR('',#4755,1.);
#1320=VECTOR('',#4756,1.);
#1321=VECTOR('',#4759,1.);
#1322=VECTOR('',#4760,1.);
#1323=VECTOR('',#4769,1.);
#1324=VECTOR('',#4772,1.);
#1325=VECTOR('',#4775,0.165);
#1326=VECTOR('',#4788,1.);
#1327=VECTOR('',#4791,1.);
#1328=VECTOR('',#4794,0.165);
#1329=VECTOR('',#4805,1.);
#1330=VECTOR('',#4808,1.);
#1331=VECTOR('',#4811,0.165);
#1332=VECTOR('',#4842,0.165);
#1333=VECTOR('',#4845,1.);
#1334=VECTOR('',#4846,1.);
#1335=VECTOR('',#4859,0.165);
#1336=VECTOR('',#4862,1.);
#1337=VECTOR('',#4863,1.);
#1338=VECTOR('',#4876,0.165);
#1339=VECTOR('',#4879,1.);
#1340=VECTOR('',#4880,1.);
#1341=VECTOR('',#4885,1.6);
#1342=VECTOR('',#4896,2.);
#1343=VECTOR('',#4903,2.);
#1344=VECTOR('',#4910,1.05);
#1345=VECTOR('',#4923,0.21);
#1346=VECTOR('',#4932,0.21);
#1347=VECTOR('',#4941,0.21);
#1348=VECTOR('',#4950,0.21);
#1349=VECTOR('',#4959,1.);
#1350=VECTOR('',#4962,1.);
#1351=VECTOR('',#4965,1.);
#1352=VECTOR('',#4966,1.);
#1353=VECTOR('',#4967,1.);
#1354=VECTOR('',#4968,1.);
#1355=VECTOR('',#4969,1.);
#1356=VECTOR('',#4972,1.);
#1357=VECTOR('',#4973,1.);
#1358=VECTOR('',#4976,1.);
#1359=VECTOR('',#4977,1.);
#1360=VECTOR('',#4978,1.);
#1361=VECTOR('',#4981,1.);
#1362=VECTOR('',#4982,1.);
#1363=VECTOR('',#4985,1.);
#1364=VECTOR('',#4986,1.);
#1365=VECTOR('',#4995,1.);
#1366=VECTOR('',#5002,1.);
#1367=VECTOR('',#5005,1.);
#1368=VECTOR('',#5008,1.);
#1369=VECTOR('',#5015,1.);
#1370=VECTOR('',#5018,1.);
#1371=VECTOR('',#5021,1.);
#1372=VECTOR('',#5022,1.);
#1373=VECTOR('',#5023,1.);
#1374=VECTOR('',#5024,1.);
#1375=VECTOR('',#5025,1.);
#1376=VECTOR('',#5028,1.);
#1377=VECTOR('',#5029,1.);
#1378=VECTOR('',#5030,1.);
#1379=VECTOR('',#5031,1.);
#1380=VECTOR('',#5032,1.);
#1381=VECTOR('',#5037,0.275);
#1382=VECTOR('',#5042,0.275);
#1383=VECTOR('',#5047,1.);
#1384=VECTOR('',#5050,1.);
#1385=VECTOR('',#5053,1.);
#1386=VECTOR('',#5054,1.);
#1387=VECTOR('',#5055,1.);
#1388=VECTOR('',#5058,1.);
#1389=VECTOR('',#5061,1.);
#1390=VECTOR('',#5062,1.);
#1391=VECTOR('',#5073,0.21);
#1392=VECTOR('',#5082,0.21);
#1393=VECTOR('',#5091,0.21);
#1394=VECTOR('',#5100,0.21);
#1395=VECTOR('',#5109,1.);
#1396=VECTOR('',#5112,1.);
#1397=VECTOR('',#5115,1.);
#1398=VECTOR('',#5116,1.);
#1399=VECTOR('',#5117,1.);
#1400=VECTOR('',#5118,1.);
#1401=VECTOR('',#5119,1.);
#1402=VECTOR('',#5122,1.);
#1403=VECTOR('',#5123,1.);
#1404=VECTOR('',#5126,1.);
#1405=VECTOR('',#5127,1.);
#1406=VECTOR('',#5128,1.);
#1407=VECTOR('',#5131,1.);
#1408=VECTOR('',#5132,1.);
#1409=VECTOR('',#5135,1.);
#1410=VECTOR('',#5136,1.);
#1411=VECTOR('',#5145,1.);
#1412=VECTOR('',#5152,1.);
#1413=VECTOR('',#5155,1.);
#1414=VECTOR('',#5158,1.);
#1415=VECTOR('',#5165,1.);
#1416=VECTOR('',#5168,1.);
#1417=VECTOR('',#5171,1.);
#1418=VECTOR('',#5172,1.);
#1419=VECTOR('',#5173,1.);
#1420=VECTOR('',#5174,1.);
#1421=VECTOR('',#5175,1.);
#1422=VECTOR('',#5178,1.);
#1423=VECTOR('',#5179,1.);
#1424=VECTOR('',#5180,1.);
#1425=VECTOR('',#5181,1.);
#1426=VECTOR('',#5182,1.);
#1427=VECTOR('',#5187,0.274999999999999);
#1428=VECTOR('',#5192,0.274999999999999);
#1429=VECTOR('',#5197,1.);
#1430=VECTOR('',#5200,1.);
#1431=VECTOR('',#5203,1.);
#1432=VECTOR('',#5204,1.);
#1433=VECTOR('',#5205,1.);
#1434=VECTOR('',#5208,1.);
#1435=VECTOR('',#5211,1.);
#1436=VECTOR('',#5212,1.);
#1437=VECTOR('',#5223,0.7);
#1438=VECTOR('',#5230,1.04);
#1439=VECTOR('',#5243,0.7);
#1440=VECTOR('',#5250,1.04);
#1441=VECTOR('',#5263,0.7);
#1442=VECTOR('',#5270,1.04);
#1443=VECTOR('',#5283,0.225);
#1444=VECTOR('',#5290,0.225);
#1445=VECTOR('',#5297,0.225);
#1446=VECTOR('',#5304,1.1);
#1447=VECTOR('',#5315,0.7);
#1448=VECTOR('',#5320,2.);
#1449=VECTOR('',#5331,1.);
#1450=VECTOR('',#5338,0.225);
#1451=VECTOR('',#5341,0.164999999999999);
#1452=VECTOR('',#5354,0.225);
#1453=VECTOR('',#5357,1.);
#1454=VECTOR('',#5358,1.);
#1455=VECTOR('',#5371,0.225);
#1456=VECTOR('',#5374,1.);
#1457=VECTOR('',#5375,1.);
#1458=VECTOR('',#5388,0.225);
#1459=VECTOR('',#5391,1.);
#1460=VECTOR('',#5392,1.);
#1461=VECTOR('',#5403,1.);
#1462=VECTOR('',#5406,1.);
#1463=VECTOR('',#5411,1.);
#1464=VECTOR('',#5412,1.);
#1465=VECTOR('',#5413,1.);
#1466=VECTOR('',#5416,1.);
#1467=VECTOR('',#5417,1.);
#1468=VECTOR('',#5418,1.);
#1469=VECTOR('',#5433,0.61);
#1470=VECTOR('',#5438,2.);
#1471=VECTOR('',#5453,0.4);
#1472=VECTOR('',#5458,0.425);
#1473=VECTOR('',#5463,0.41);
#1474=VECTOR('',#5472,0.26);
#1475=VECTOR('',#5477,0.25);
#1476=VECTOR('',#5482,0.225);
#1477=VECTOR('',#5487,1.);
#1478=VECTOR('',#5488,1.);
#1479=VECTOR('',#5489,1.);
#1480=VECTOR('',#5490,1.);
#1481=VECTOR('',#5493,1.);
#1482=VECTOR('',#5494,1.);
#1483=VECTOR('',#5495,1.);
#1484=VECTOR('',#5498,1.);
#1485=VECTOR('',#5499,1.);
#1486=VECTOR('',#5500,1.);
#1487=VECTOR('',#5503,1.);
#1488=VECTOR('',#5504,1.);
#1489=VECTOR('',#5505,1.);
#1490=VECTOR('',#5508,1.);
#1491=VECTOR('',#5509,1.);
#1492=VECTOR('',#5510,1.);
#1493=VECTOR('',#5513,1.);
#1494=VECTOR('',#5514,1.);
#1495=VECTOR('',#5527,1.);
#1496=VECTOR('',#5528,1.);
#1497=VECTOR('',#5529,1.);
#1498=VECTOR('',#5532,1.);
#1499=VECTOR('',#5533,1.);
#1500=VECTOR('',#5534,1.);
#1501=VECTOR('',#5539,1.);
#1502=VECTOR('',#5540,1.);
#1503=VECTOR('',#5543,1.);
#1504=VECTOR('',#5544,1.);
#1505=VECTOR('',#5557,1.05);
#1506=VECTOR('',#5566,1.);
#1507=VECTOR('',#5575,1.05);
#1508=VECTOR('',#5584,1.);
#1509=VECTOR('',#5593,1.05);
#1510=VECTOR('',#5600,0.9);
#1511=VECTOR('',#5607,1.);
#1512=VECTOR('',#5610,1.);
#1513=VECTOR('',#5613,1.);
#1514=VECTOR('',#5614,1.);
#1515=VECTOR('',#5615,1.);
#1516=VECTOR('',#5622,1.);
#1517=VECTOR('',#5625,1.);
#1518=VECTOR('',#5626,1.);
#1519=VECTOR('',#5637,0.895);
#1520=VECTOR('',#5644,0.605);
#1521=VECTOR('',#5655,1.);
#1522=VECTOR('',#5662,0.210000000000001);
#1523=VECTOR('',#5665,1.);
#1524=VECTOR('',#5670,0.605);
#1525=VECTOR('',#5671,0.605);
#1526=VECTOR('',#5678,1.1);
#1527=VECTOR('',#5679,1.1);
#1528=VECTOR('',#5690,1.);
#1529=VECTOR('',#5697,0.210000000000001);
#1530=VECTOR('',#5700,1.);
#1531=VECTOR('',#5705,0.605);
#1532=VECTOR('',#5706,0.605);
#1533=VECTOR('',#5713,1.1);
#1534=VECTOR('',#5714,1.1);
#1535=VECTOR('',#5727,0.375);
#1536=VECTOR('',#5736,0.225);
#1537=VECTOR('',#5743,1.4);
#1538=VECTOR('',#5756,0.165);
#1539=VECTOR('',#5765,0.55);
#1540=VECTOR('',#5772,0.6);
#1541=VECTOR('',#5779,0.55);
#1542=VECTOR('',#5786,1.);
#1543=VECTOR('',#5787,1.);
#1544=VECTOR('',#5788,1.);
#1545=VECTOR('',#5789,1.);
#1546=VECTOR('',#5792,1.);
#1547=VECTOR('',#5793,1.);
#1548=VECTOR('',#5794,1.);
#1549=VECTOR('',#5797,1.);
#1550=VECTOR('',#5798,1.);
#1551=VECTOR('',#5799,1.);
#1552=VECTOR('',#5802,1.);
#1553=VECTOR('',#5803,1.);
#1554=VECTOR('',#5804,1.);
#1555=VECTOR('',#5807,1.);
#1556=VECTOR('',#5808,1.);
#1557=VECTOR('',#5809,1.);
#1558=VECTOR('',#5812,1.);
#1559=VECTOR('',#5813,1.);
#1560=VECTOR('',#5824,0.235);
#1561=VECTOR('',#5829,0.25);
#1562=VECTOR('',#5834,0.2125);
#1563=VECTOR('',#5847,0.325);
#1564=VECTOR('',#5852,0.35);
#1565=VECTOR('',#5857,0.335);
#1566=VECTOR('',#5866,0.21);
#1567=VECTOR('',#5871,0.2);
#1568=VECTOR('',#5876,0.18);
#1569=VECTOR('',#5881,1.);
#1570=VECTOR('',#5882,1.);
#1571=VECTOR('',#5883,1.);
#1572=VECTOR('',#5884,1.);
#1573=VECTOR('',#5887,1.);
#1574=VECTOR('',#5888,1.);
#1575=VECTOR('',#5889,1.);
#1576=VECTOR('',#5892,1.);
#1577=VECTOR('',#5893,1.);
#1578=VECTOR('',#5894,1.);
#1579=VECTOR('',#5897,1.);
#1580=VECTOR('',#5898,1.);
#1581=VECTOR('',#5899,1.);
#1582=VECTOR('',#5902,1.);
#1583=VECTOR('',#5903,1.);
#1584=VECTOR('',#5904,1.);
#1585=VECTOR('',#5907,1.);
#1586=VECTOR('',#5908,1.);
#1587=CIRCLE('',#4211,0.274999999999999);
#1588=CIRCLE('',#4212,0.274999999999999);
#1589=CIRCLE('',#4214,0.275);
#1590=CIRCLE('',#4215,0.275);
#1591=CIRCLE('',#4217,0.275);
#1592=CIRCLE('',#4218,0.275);
#1593=CIRCLE('',#4220,0.274999999999999);
#1594=CIRCLE('',#4221,0.274999999999999);
#1595=CIRCLE('',#4230,0.165);
#1596=CIRCLE('',#4231,0.165);
#1597=CIRCLE('',#4232,0.165);
#1598=CIRCLE('',#4233,0.165);
#1599=CIRCLE('',#4235,1.6);
#1600=CIRCLE('',#4236,1.6);
#1601=CIRCLE('',#4238,0.165);
#1602=CIRCLE('',#4239,0.165);
#1603=CIRCLE('',#4240,0.165);
#1604=CIRCLE('',#4241,0.165);
#1605=CIRCLE('',#4243,1.6);
#1606=CIRCLE('',#4245,0.165);
#1607=CIRCLE('',#4246,0.165);
#1608=CIRCLE('',#4247,0.165);
#1609=CIRCLE('',#4248,0.165);
#1610=CIRCLE('',#4250,1.6);
#1611=CIRCLE('',#4252,2.);
#1612=CIRCLE('',#4253,1.6);
#1613=CIRCLE('',#4254,1.6);
#1614=CIRCLE('',#4255,1.6);
#1615=CIRCLE('',#4257,1.6);
#1616=CIRCLE('',#4258,0.165);
#1617=CIRCLE('',#4259,1.6);
#1618=CIRCLE('',#4261,0.165);
#1619=CIRCLE('',#4262,0.165);
#1620=CIRCLE('',#4263,0.165);
#1621=CIRCLE('',#4265,1.6);
#1622=CIRCLE('',#4266,0.165);
#1623=CIRCLE('',#4268,0.165);
#1624=CIRCLE('',#4269,0.165);
#1625=CIRCLE('',#4270,0.165);
#1626=CIRCLE('',#4272,1.6);
#1627=CIRCLE('',#4273,0.165);
#1628=CIRCLE('',#4275,0.165);
#1629=CIRCLE('',#4276,0.165);
#1630=CIRCLE('',#4277,0.165);
#1631=CIRCLE('',#4279,1.6);
#1632=CIRCLE('',#4280,1.6);
#1633=CIRCLE('',#4281,1.6);
#1634=CIRCLE('',#4283,2.);
#1635=CIRCLE('',#4285,2.);
#1636=CIRCLE('',#4287,2.);
#1637=CIRCLE('',#4289,1.05);
#1638=CIRCLE('',#4290,1.05);
#1639=CIRCLE('',#4295,0.21);
#1640=CIRCLE('',#4296,0.21);
#1641=CIRCLE('',#4299,0.21);
#1642=CIRCLE('',#4300,0.21);
#1643=CIRCLE('',#4303,0.21);
#1644=CIRCLE('',#4304,0.21);
#1645=CIRCLE('',#4307,0.21);
#1646=CIRCLE('',#4308,0.21);
#1647=CIRCLE('',#4311,1.6);
#1648=CIRCLE('',#4312,1.6);
#1649=CIRCLE('',#4322,0.475);
#1650=CIRCLE('',#4323,0.275);
#1651=CIRCLE('',#4325,0.475);
#1652=CIRCLE('',#4327,0.475);
#1653=CIRCLE('',#4328,0.275);
#1654=CIRCLE('',#4330,0.475);
#1655=CIRCLE('',#4334,0.275);
#1656=CIRCLE('',#4336,0.275);
#1657=CIRCLE('',#4338,1.6);
#1658=CIRCLE('',#4339,1.6);
#1659=CIRCLE('',#4347,0.21);
#1660=CIRCLE('',#4348,0.21);
#1661=CIRCLE('',#4351,0.21);
#1662=CIRCLE('',#4352,0.21);
#1663=CIRCLE('',#4355,0.21);
#1664=CIRCLE('',#4356,0.21);
#1665=CIRCLE('',#4359,0.21);
#1666=CIRCLE('',#4360,0.21);
#1667=CIRCLE('',#4363,1.6);
#1668=CIRCLE('',#4364,1.6);
#1669=CIRCLE('',#4374,0.475000000000001);
#1670=CIRCLE('',#4375,0.274999999999999);
#1671=CIRCLE('',#4377,0.475000000000001);
#1672=CIRCLE('',#4379,0.475000000000001);
#1673=CIRCLE('',#4380,0.274999999999999);
#1674=CIRCLE('',#4382,0.475000000000001);
#1675=CIRCLE('',#4386,0.274999999999999);
#1676=CIRCLE('',#4388,0.274999999999999);
#1677=CIRCLE('',#4390,1.6);
#1678=CIRCLE('',#4391,1.6);
#1679=CIRCLE('',#4399,0.7);
#1680=CIRCLE('',#4400,0.7);
#1681=CIRCLE('',#4402,1.04);
#1682=CIRCLE('',#4403,1.04);
#1683=CIRCLE('',#4408,0.7);
#1684=CIRCLE('',#4409,0.7);
#1685=CIRCLE('',#4411,1.04);
#1686=CIRCLE('',#4412,1.04);
#1687=CIRCLE('',#4417,0.7);
#1688=CIRCLE('',#4418,0.7);
#1689=CIRCLE('',#4420,1.04);
#1690=CIRCLE('',#4421,1.04);
#1691=CIRCLE('',#4426,0.225);
#1692=CIRCLE('',#4427,0.225);
#1693=CIRCLE('',#4429,0.225);
#1694=CIRCLE('',#4430,0.225);
#1695=CIRCLE('',#4432,0.225);
#1696=CIRCLE('',#4433,0.225);
#1697=CIRCLE('',#4435,1.1);
#1698=CIRCLE('',#4436,1.1);
#1699=CIRCLE('',#4438,0.7);
#1700=CIRCLE('',#4440,0.7);
#1701=CIRCLE('',#4442,2.);
#1702=CIRCLE('',#4443,2.);
#1703=CIRCLE('',#4448,0.225);
#1704=CIRCLE('',#4450,0.225);
#1705=CIRCLE('',#4452,0.164999999999999);
#1706=CIRCLE('',#4454,1.5);
#1707=CIRCLE('',#4455,0.225);
#1708=CIRCLE('',#4457,0.225);
#1709=CIRCLE('',#4458,0.225);
#1710=CIRCLE('',#4459,0.225);
#1711=CIRCLE('',#4461,1.5);
#1712=CIRCLE('',#4462,0.225);
#1713=CIRCLE('',#4464,0.225);
#1714=CIRCLE('',#4465,0.225);
#1715=CIRCLE('',#4466,0.225);
#1716=CIRCLE('',#4468,1.5);
#1717=CIRCLE('',#4469,0.225);
#1718=CIRCLE('',#4471,0.225);
#1719=CIRCLE('',#4472,0.225);
#1720=CIRCLE('',#4473,0.225);
#1721=CIRCLE('',#4475,1.5);
#1722=CIRCLE('',#4476,1.5);
#1723=CIRCLE('',#4477,1.5);
#1724=CIRCLE('',#4478,1.5);
#1725=CIRCLE('',#4479,1.5);
#1726=CIRCLE('',#4483,2.);
#1727=CIRCLE('',#4484,0.61);
#1728=CIRCLE('',#4486,0.61);
#1729=CIRCLE('',#4487,0.61);
#1730=CIRCLE('',#4489,0.61);
#1731=CIRCLE('',#4491,2.);
#1732=CIRCLE('',#4495,0.375);
#1733=CIRCLE('',#4497,0.425);
#1734=CIRCLE('',#4499,0.425);
#1735=CIRCLE('',#4501,0.395);
#1736=CIRCLE('',#4503,0.27);
#1737=CIRCLE('',#4505,0.24505);
#1738=CIRCLE('',#4507,0.24505);
#1739=CIRCLE('',#4509,0.2);
#1740=CIRCLE('',#4522,0.9);
#1741=CIRCLE('',#4525,0.9);
#1742=CIRCLE('',#4529,1.05);
#1743=CIRCLE('',#4530,0.9);
#1744=CIRCLE('',#4532,1.05);
#1745=CIRCLE('',#4534,1.);
#1746=CIRCLE('',#4536,1.);
#1747=CIRCLE('',#4538,1.05);
#1748=CIRCLE('',#4540,1.05);
#1749=CIRCLE('',#4542,1.);
#1750=CIRCLE('',#4544,1.);
#1751=CIRCLE('',#4546,1.05);
#1752=CIRCLE('',#4548,1.05);
#1753=CIRCLE('',#4550,0.9);
#1754=CIRCLE('',#4554,0.895);
#1755=CIRCLE('',#4555,0.605);
#1756=CIRCLE('',#4558,0.895);
#1757=CIRCLE('',#4559,0.605);
#1758=CIRCLE('',#4562,0.895);
#1759=CIRCLE('',#4563,0.605);
#1760=CIRCLE('',#4565,0.895);
#1761=CIRCLE('',#4567,0.605);
#1762=CIRCLE('',#4574,0.210000000000001);
#1763=CIRCLE('',#4576,0.210000000000001);
#1764=CIRCLE('',#4579,0.605);
#1765=CIRCLE('',#4580,0.605);
#1766=CIRCLE('',#4582,1.1);
#1767=CIRCLE('',#4583,1.1);
#1768=CIRCLE('',#4588,0.210000000000001);
#1769=CIRCLE('',#4590,0.210000000000001);
#1770=CIRCLE('',#4593,0.605);
#1771=CIRCLE('',#4594,0.605);
#1772=CIRCLE('',#4596,1.1);
#1773=CIRCLE('',#4597,1.1);
#1774=CIRCLE('',#4602,0.375);
#1775=CIRCLE('',#4603,0.375);
#1776=CIRCLE('',#4605,0.225);
#1777=CIRCLE('',#4607,0.225);
#1778=CIRCLE('',#4609,1.4);
#1779=CIRCLE('',#4610,1.4);
#1780=CIRCLE('',#4615,0.165);
#1781=CIRCLE('',#4616,0.165);
#1782=CIRCLE('',#4619,0.6);
#1783=CIRCLE('',#4620,0.5);
#1784=CIRCLE('',#4622,0.6);
#1785=CIRCLE('',#4625,0.5);
#1786=CIRCLE('',#4636,0.22);
#1787=CIRCLE('',#4638,0.24505);
#1788=CIRCLE('',#4640,0.24505);
#1789=CIRCLE('',#4642,0.175);
#1790=CIRCLE('',#4646,0.3);
#1791=CIRCLE('',#4648,0.35);
#1792=CIRCLE('',#4650,0.35);
#1793=CIRCLE('',#4652,0.32);
#1794=CIRCLE('',#4654,0.22);
#1795=CIRCLE('',#4656,0.1954);
#1796=CIRCLE('',#4658,0.1954);
#1797=CIRCLE('',#4660,0.16);
#1798=VERTEX_POINT('',#5991);
#1799=VERTEX_POINT('',#5993);
#1800=VERTEX_POINT('',#5997);
#1801=VERTEX_POINT('',#5999);
#1802=VERTEX_POINT('',#6003);
#1803=VERTEX_POINT('',#6005);
#1804=VERTEX_POINT('',#6009);
#1805=VERTEX_POINT('',#6011);
#1806=VERTEX_POINT('',#6015);
#1807=VERTEX_POINT('',#6016);
#1808=VERTEX_POINT('',#6018);
#1809=VERTEX_POINT('',#6020);
#1810=VERTEX_POINT('',#6024);
#1811=VERTEX_POINT('',#6026);
#1812=VERTEX_POINT('',#6030);
#1813=VERTEX_POINT('',#6032);
#1814=VERTEX_POINT('',#6042);
#1815=VERTEX_POINT('',#6043);
#1816=VERTEX_POINT('',#6045);
#1817=VERTEX_POINT('',#6047);
#1818=VERTEX_POINT('',#6049);
#1819=VERTEX_POINT('',#6051);
#1820=VERTEX_POINT('',#6056);
#1821=VERTEX_POINT('',#6060);
#1822=VERTEX_POINT('',#6061);
#1823=VERTEX_POINT('',#6063);
#1824=VERTEX_POINT('',#6065);
#1825=VERTEX_POINT('',#6067);
#1826=VERTEX_POINT('',#6069);
#1827=VERTEX_POINT('',#6076);
#1828=VERTEX_POINT('',#6077);
#1829=VERTEX_POINT('',#6079);
#1830=VERTEX_POINT('',#6081);
#1831=VERTEX_POINT('',#6083);
#1832=VERTEX_POINT('',#6085);
#1833=VERTEX_POINT('',#6092);
#1834=VERTEX_POINT('',#6098);
#1835=VERTEX_POINT('',#6099);
#1836=VERTEX_POINT('',#6101);
#1837=VERTEX_POINT('',#6105);
#1838=VERTEX_POINT('',#6107);
#1839=VERTEX_POINT('',#6109);
#1840=VERTEX_POINT('',#6112);
#1841=VERTEX_POINT('',#6116);
#1842=VERTEX_POINT('',#6117);
#1843=VERTEX_POINT('',#6121);
#1844=VERTEX_POINT('',#6123);
#1845=VERTEX_POINT('',#6125);
#1846=VERTEX_POINT('',#6128);
#1847=VERTEX_POINT('',#6132);
#1848=VERTEX_POINT('',#6133);
#1849=VERTEX_POINT('',#6137);
#1850=VERTEX_POINT('',#6139);
#1851=VERTEX_POINT('',#6141);
#1852=VERTEX_POINT('',#6144);
#1853=VERTEX_POINT('',#6153);
#1854=VERTEX_POINT('',#6157);
#1855=VERTEX_POINT('',#6160);
#1856=VERTEX_POINT('',#6164);
#1857=VERTEX_POINT('',#6166);
#1858=VERTEX_POINT('',#6173);
#1859=VERTEX_POINT('',#6175);
#1860=VERTEX_POINT('',#6180);
#1861=VERTEX_POINT('',#6182);
#1862=VERTEX_POINT('',#6187);
#1863=VERTEX_POINT('',#6189);
#1864=VERTEX_POINT('',#6194);
#1865=VERTEX_POINT('',#6196);
#1866=VERTEX_POINT('',#6201);
#1867=VERTEX_POINT('',#6202);
#1868=VERTEX_POINT('',#6204);
#1869=VERTEX_POINT('',#6206);
#1870=VERTEX_POINT('',#6210);
#1871=VERTEX_POINT('',#6212);
#1872=VERTEX_POINT('',#6214);
#1873=VERTEX_POINT('',#6216);
#1874=VERTEX_POINT('',#6220);
#1875=VERTEX_POINT('',#6224);
#1876=VERTEX_POINT('',#6226);
#1877=VERTEX_POINT('',#6230);
#1878=VERTEX_POINT('',#6240);
#1879=VERTEX_POINT('',#6241);
#1880=VERTEX_POINT('',#6244);
#1881=VERTEX_POINT('',#6247);
#1882=VERTEX_POINT('',#6249);
#1883=VERTEX_POINT('',#6253);
#1884=VERTEX_POINT('',#6254);
#1885=VERTEX_POINT('',#6257);
#1886=VERTEX_POINT('',#6260);
#1887=VERTEX_POINT('',#6262);
#1888=VERTEX_POINT('',#6266);
#1889=VERTEX_POINT('',#6268);
#1890=VERTEX_POINT('',#6270);
#1891=VERTEX_POINT('',#6272);
#1892=VERTEX_POINT('',#6276);
#1893=VERTEX_POINT('',#6278);
#1894=VERTEX_POINT('',#6280);
#1895=VERTEX_POINT('',#6282);
#1896=VERTEX_POINT('',#6286);
#1897=VERTEX_POINT('',#6290);
#1898=VERTEX_POINT('',#6294);
#1899=VERTEX_POINT('',#6295);
#1900=VERTEX_POINT('',#6297);
#1901=VERTEX_POINT('',#6299);
#1902=VERTEX_POINT('',#6315);
#1903=VERTEX_POINT('',#6317);
#1904=VERTEX_POINT('',#6322);
#1905=VERTEX_POINT('',#6324);
#1906=VERTEX_POINT('',#6329);
#1907=VERTEX_POINT('',#6331);
#1908=VERTEX_POINT('',#6336);
#1909=VERTEX_POINT('',#6338);
#1910=VERTEX_POINT('',#6343);
#1911=VERTEX_POINT('',#6344);
#1912=VERTEX_POINT('',#6346);
#1913=VERTEX_POINT('',#6348);
#1914=VERTEX_POINT('',#6352);
#1915=VERTEX_POINT('',#6354);
#1916=VERTEX_POINT('',#6356);
#1917=VERTEX_POINT('',#6358);
#1918=VERTEX_POINT('',#6362);
#1919=VERTEX_POINT('',#6366);
#1920=VERTEX_POINT('',#6368);
#1921=VERTEX_POINT('',#6372);
#1922=VERTEX_POINT('',#6382);
#1923=VERTEX_POINT('',#6383);
#1924=VERTEX_POINT('',#6386);
#1925=VERTEX_POINT('',#6389);
#1926=VERTEX_POINT('',#6391);
#1927=VERTEX_POINT('',#6395);
#1928=VERTEX_POINT('',#6396);
#1929=VERTEX_POINT('',#6399);
#1930=VERTEX_POINT('',#6402);
#1931=VERTEX_POINT('',#6404);
#1932=VERTEX_POINT('',#6408);
#1933=VERTEX_POINT('',#6410);
#1934=VERTEX_POINT('',#6412);
#1935=VERTEX_POINT('',#6414);
#1936=VERTEX_POINT('',#6418);
#1937=VERTEX_POINT('',#6420);
#1938=VERTEX_POINT('',#6422);
#1939=VERTEX_POINT('',#6424);
#1940=VERTEX_POINT('',#6428);
#1941=VERTEX_POINT('',#6432);
#1942=VERTEX_POINT('',#6436);
#1943=VERTEX_POINT('',#6437);
#1944=VERTEX_POINT('',#6439);
#1945=VERTEX_POINT('',#6441);
#1946=VERTEX_POINT('',#6457);
#1947=VERTEX_POINT('',#6459);
#1948=VERTEX_POINT('',#6463);
#1949=VERTEX_POINT('',#6465);
#1950=VERTEX_POINT('',#6472);
#1951=VERTEX_POINT('',#6474);
#1952=VERTEX_POINT('',#6478);
#1953=VERTEX_POINT('',#6480);
#1954=VERTEX_POINT('',#6487);
#1955=VERTEX_POINT('',#6489);
#1956=VERTEX_POINT('',#6493);
#1957=VERTEX_POINT('',#6495);
#1958=VERTEX_POINT('',#6502);
#1959=VERTEX_POINT('',#6504);
#1960=VERTEX_POINT('',#6508);
#1961=VERTEX_POINT('',#6510);
#1962=VERTEX_POINT('',#6514);
#1963=VERTEX_POINT('',#6516);
#1964=VERTEX_POINT('',#6520);
#1965=VERTEX_POINT('',#6522);
#1966=VERTEX_POINT('',#6526);
#1967=VERTEX_POINT('',#6529);
#1968=VERTEX_POINT('',#6533);
#1969=VERTEX_POINT('',#6535);
#1970=VERTEX_POINT('',#6542);
#1971=VERTEX_POINT('',#6543);
#1972=VERTEX_POINT('',#6547);
#1973=VERTEX_POINT('',#6549);
#1974=VERTEX_POINT('',#6586);
#1975=VERTEX_POINT('',#6587);
#1976=VERTEX_POINT('',#6628);
#1977=VERTEX_POINT('',#6632);
#1978=VERTEX_POINT('',#6633);
#1979=VERTEX_POINT('',#6637);
#1980=VERTEX_POINT('',#6639);
#1981=VERTEX_POINT('',#6641);
#1982=VERTEX_POINT('',#6644);
#1983=VERTEX_POINT('',#6648);
#1984=VERTEX_POINT('',#6649);
#1985=VERTEX_POINT('',#6653);
#1986=VERTEX_POINT('',#6655);
#1987=VERTEX_POINT('',#6657);
#1988=VERTEX_POINT('',#6660);
#1989=VERTEX_POINT('',#6664);
#1990=VERTEX_POINT('',#6665);
#1991=VERTEX_POINT('',#6669);
#1992=VERTEX_POINT('',#6671);
#1993=VERTEX_POINT('',#6673);
#1994=VERTEX_POINT('',#6676);
#1995=VERTEX_POINT('',#6682);
#1996=VERTEX_POINT('',#6684);
#1997=VERTEX_POINT('',#6686);
#1998=VERTEX_POINT('',#6688);
#1999=VERTEX_POINT('',#6692);
#2000=VERTEX_POINT('',#6693);
#2001=VERTEX_POINT('',#6698);
#2002=VERTEX_POINT('',#6699);
#2003=VERTEX_POINT('',#6704);
#2004=VERTEX_POINT('',#6708);
#2005=VERTEX_POINT('',#6712);
#2006=VERTEX_POINT('',#6716);
#2007=VERTEX_POINT('',#6722);
#2008=VERTEX_POINT('',#6725);
#2009=VERTEX_POINT('',#6729);
#2010=VERTEX_POINT('',#6733);
#2011=VERTEX_POINT('',#6737);
#2012=VERTEX_POINT('',#6740);
#2013=VERTEX_POINT('',#6744);
#2014=VERTEX_POINT('',#6748);
#2015=VERTEX_POINT('',#6753);
#2016=VERTEX_POINT('',#6754);
#2017=VERTEX_POINT('',#6756);
#2018=VERTEX_POINT('',#6758);
#2019=VERTEX_POINT('',#6762);
#2020=VERTEX_POINT('',#6764);
#2021=VERTEX_POINT('',#6768);
#2022=VERTEX_POINT('',#6770);
#2023=VERTEX_POINT('',#6774);
#2024=VERTEX_POINT('',#6776);
#2025=VERTEX_POINT('',#6780);
#2026=VERTEX_POINT('',#6782);
#2027=VERTEX_POINT('',#6793);
#2028=VERTEX_POINT('',#6794);
#2029=VERTEX_POINT('',#6796);
#2030=VERTEX_POINT('',#6798);
#2031=VERTEX_POINT('',#6802);
#2032=VERTEX_POINT('',#6804);
#2033=VERTEX_POINT('',#6808);
#2034=VERTEX_POINT('',#6810);
#2035=VERTEX_POINT('',#6818);
#2036=VERTEX_POINT('',#6820);
#2037=VERTEX_POINT('',#6823);
#2038=VERTEX_POINT('',#6827);
#2039=VERTEX_POINT('',#6830);
#2040=VERTEX_POINT('',#6834);
#2041=VERTEX_POINT('',#6837);
#2042=VERTEX_POINT('',#6841);
#2043=VERTEX_POINT('',#6844);
#2044=VERTEX_POINT('',#6848);
#2045=VERTEX_POINT('',#6851);
#2046=VERTEX_POINT('',#6855);
#2047=VERTEX_POINT('',#6861);
#2048=VERTEX_POINT('',#6862);
#2049=VERTEX_POINT('',#6864);
#2050=VERTEX_POINT('',#6866);
#2051=VERTEX_POINT('',#6870);
#2052=VERTEX_POINT('',#6872);
#2053=VERTEX_POINT('',#6876);
#2054=VERTEX_POINT('',#6878);
#2055=VERTEX_POINT('',#6885);
#2056=VERTEX_POINT('',#6887);
#2057=VERTEX_POINT('',#6890);
#2058=VERTEX_POINT('',#6894);
#2059=VERTEX_POINT('',#6903);
#2060=VERTEX_POINT('',#6904);
#2061=VERTEX_POINT('',#6908);
#2062=VERTEX_POINT('',#6909);
#2063=VERTEX_POINT('',#6916);
#2064=VERTEX_POINT('',#6918);
#2065=VERTEX_POINT('',#6937);
#2066=VERTEX_POINT('',#6939);
#2067=VERTEX_POINT('',#6950);
#2068=VERTEX_POINT('',#6982);
#2069=VERTEX_POINT('',#6985);
#2070=VERTEX_POINT('',#6989);
#2071=VERTEX_POINT('',#6992);
#2072=VERTEX_POINT('',#6999);
#2073=VERTEX_POINT('',#7000);
#2074=VERTEX_POINT('',#7004);
#2075=VERTEX_POINT('',#7005);
#2076=VERTEX_POINT('',#7012);
#2077=VERTEX_POINT('',#7014);
#2078=VERTEX_POINT('',#7033);
#2079=VERTEX_POINT('',#7035);
#2080=VERTEX_POINT('',#7046);
#2081=VERTEX_POINT('',#7078);
#2082=VERTEX_POINT('',#7081);
#2083=VERTEX_POINT('',#7085);
#2084=VERTEX_POINT('',#7088);
#2085=VERTEX_POINT('',#7095);
#2086=VERTEX_POINT('',#7097);
#2087=VERTEX_POINT('',#7101);
#2088=VERTEX_POINT('',#7104);
#2089=VERTEX_POINT('',#7108);
#2090=VERTEX_POINT('',#7110);
#2091=VERTEX_POINT('',#7117);
#2092=VERTEX_POINT('',#7119);
#2093=VERTEX_POINT('',#7124);
#2094=VERTEX_POINT('',#7126);
#2095=VERTEX_POINT('',#7130);
#2096=VERTEX_POINT('',#7135);
#2097=VERTEX_POINT('',#7141);
#2098=VERTEX_POINT('',#7142);
#2099=VERTEX_POINT('',#7144);
#2100=VERTEX_POINT('',#7146);
#2101=VERTEX_POINT('',#7150);
#2102=VERTEX_POINT('',#7152);
#2103=VERTEX_POINT('',#7156);
#2104=VERTEX_POINT('',#7158);
#2105=VERTEX_POINT('',#7162);
#2106=VERTEX_POINT('',#7164);
#2107=VERTEX_POINT('',#7168);
#2108=VERTEX_POINT('',#7170);
#2109=VERTEX_POINT('',#7178);
#2110=VERTEX_POINT('',#7181);
#2111=VERTEX_POINT('',#7185);
#2112=VERTEX_POINT('',#7189);
#2113=VERTEX_POINT('',#7195);
#2114=VERTEX_POINT('',#7198);
#2115=VERTEX_POINT('',#7202);
#2116=VERTEX_POINT('',#7206);
#2117=VERTEX_POINT('',#7210);
#2118=VERTEX_POINT('',#7213);
#2119=VERTEX_POINT('',#7217);
#2120=VERTEX_POINT('',#7221);
#2121=VERTEX_POINT('',#7226);
#2122=VERTEX_POINT('',#7227);
#2123=VERTEX_POINT('',#7229);
#2124=VERTEX_POINT('',#7231);
#2125=VERTEX_POINT('',#7235);
#2126=VERTEX_POINT('',#7237);
#2127=VERTEX_POINT('',#7241);
#2128=VERTEX_POINT('',#7243);
#2129=VERTEX_POINT('',#7247);
#2130=VERTEX_POINT('',#7249);
#2131=VERTEX_POINT('',#7253);
#2132=VERTEX_POINT('',#7255);
#2133=EDGE_CURVE('',#1798,#1798,#1587,.T.);
#2134=EDGE_CURVE('',#1798,#1799,#1027,.T.);
#2135=EDGE_CURVE('',#1799,#1799,#1588,.T.);
#2136=EDGE_CURVE('',#1800,#1800,#1589,.T.);
#2137=EDGE_CURVE('',#1800,#1801,#1028,.T.);
#2138=EDGE_CURVE('',#1801,#1801,#1590,.T.);
#2139=EDGE_CURVE('',#1802,#1802,#1591,.T.);
#2140=EDGE_CURVE('',#1802,#1803,#1029,.T.);
#2141=EDGE_CURVE('',#1803,#1803,#1592,.T.);
#2142=EDGE_CURVE('',#1804,#1804,#1593,.T.);
#2143=EDGE_CURVE('',#1804,#1805,#1030,.T.);
#2144=EDGE_CURVE('',#1805,#1805,#1594,.T.);
#2145=EDGE_CURVE('',#1806,#1807,#1031,.T.);
#2146=EDGE_CURVE('',#1807,#1808,#1032,.T.);
#2147=EDGE_CURVE('',#1809,#1808,#1033,.T.);
#2148=EDGE_CURVE('',#1806,#1809,#1034,.T.);
#2149=EDGE_CURVE('',#1810,#1806,#1035,.T.);
#2150=EDGE_CURVE('',#1811,#1809,#1036,.T.);
#2151=EDGE_CURVE('',#1810,#1811,#1037,.T.);
#2152=EDGE_CURVE('',#1812,#1810,#1038,.T.);
#2153=EDGE_CURVE('',#1813,#1811,#1039,.T.);
#2154=EDGE_CURVE('',#1812,#1813,#1040,.T.);
#2155=EDGE_CURVE('',#1807,#1812,#1041,.T.);
#2156=EDGE_CURVE('',#1808,#1813,#1042,.T.);
#2157=EDGE_CURVE('',#1814,#1815,#1043,.T.);
#2158=EDGE_CURVE('',#1816,#1814,#1595,.T.);
#2159=EDGE_CURVE('',#1817,#1816,#1044,.T.);
#2160=EDGE_CURVE('',#1818,#1817,#1596,.T.);
#2161=EDGE_CURVE('',#1818,#1819,#1045,.T.);
#2162=EDGE_CURVE('',#1819,#1819,#1597,.T.);
#2163=EDGE_CURVE('',#1815,#1818,#1598,.T.);
#2164=EDGE_CURVE('',#1816,#1820,#1599,.T.);
#2165=EDGE_CURVE('',#1820,#1814,#1600,.T.);
#2166=EDGE_CURVE('',#1821,#1822,#1046,.T.);
#2167=EDGE_CURVE('',#1823,#1821,#1601,.T.);
#2168=EDGE_CURVE('',#1824,#1823,#1047,.T.);
#2169=EDGE_CURVE('',#1825,#1824,#1602,.T.);
#2170=EDGE_CURVE('',#1825,#1826,#1048,.T.);
#2171=EDGE_CURVE('',#1826,#1826,#1603,.T.);
#2172=EDGE_CURVE('',#1822,#1825,#1604,.T.);
#2173=EDGE_CURVE('',#1823,#1821,#1605,.T.);
#2174=EDGE_CURVE('',#1827,#1828,#1049,.T.);
#2175=EDGE_CURVE('',#1829,#1827,#1606,.T.);
#2176=EDGE_CURVE('',#1830,#1829,#1050,.T.);
#2177=EDGE_CURVE('',#1831,#1830,#1607,.T.);
#2178=EDGE_CURVE('',#1831,#1832,#1051,.T.);
#2179=EDGE_CURVE('',#1832,#1832,#1608,.T.);
#2180=EDGE_CURVE('',#1828,#1831,#1609,.T.);
#2181=EDGE_CURVE('',#1829,#1827,#1610,.T.);
#2182=EDGE_CURVE('',#1833,#1833,#1611,.T.);
#2183=EDGE_CURVE('',#1822,#1817,#1612,.T.);
#2184=EDGE_CURVE('',#1828,#1824,#1613,.T.);
#2185=EDGE_CURVE('',#1815,#1830,#1614,.T.);
#2186=EDGE_CURVE('',#1834,#1835,#1615,.T.);
#2187=EDGE_CURVE('',#1836,#1834,#1616,.T.);
#2188=EDGE_CURVE('',#1835,#1836,#1617,.T.);
#2189=EDGE_CURVE('',#1837,#1837,#1618,.T.);
#2190=EDGE_CURVE('',#1837,#1838,#1052,.T.);
#2191=EDGE_CURVE('',#1839,#1838,#1619,.T.);
#2192=EDGE_CURVE('',#1836,#1839,#1053,.T.);
#2193=EDGE_CURVE('',#1840,#1834,#1054,.T.);
#2194=EDGE_CURVE('',#1838,#1840,#1620,.T.);
#2195=EDGE_CURVE('',#1841,#1842,#1621,.T.);
#2196=EDGE_CURVE('',#1842,#1841,#1622,.T.);
#2197=EDGE_CURVE('',#1843,#1843,#1623,.T.);
#2198=EDGE_CURVE('',#1843,#1844,#1055,.T.);
#2199=EDGE_CURVE('',#1845,#1844,#1624,.T.);
#2200=EDGE_CURVE('',#1842,#1845,#1056,.T.);
#2201=EDGE_CURVE('',#1846,#1841,#1057,.T.);
#2202=EDGE_CURVE('',#1844,#1846,#1625,.T.);
#2203=EDGE_CURVE('',#1847,#1848,#1626,.T.);
#2204=EDGE_CURVE('',#1848,#1847,#1627,.T.);
#2205=EDGE_CURVE('',#1849,#1849,#1628,.T.);
#2206=EDGE_CURVE('',#1849,#1850,#1058,.T.);
#2207=EDGE_CURVE('',#1851,#1850,#1629,.T.);
#2208=EDGE_CURVE('',#1848,#1851,#1059,.T.);
#2209=EDGE_CURVE('',#1852,#1847,#1060,.T.);
#2210=EDGE_CURVE('',#1850,#1852,#1630,.T.);
#2211=EDGE_CURVE('',#1820,#1835,#1061,.T.);
#2212=EDGE_CURVE('',#1839,#1846,#1631,.T.);
#2213=EDGE_CURVE('',#1845,#1852,#1632,.T.);
#2214=EDGE_CURVE('',#1851,#1840,#1633,.T.);
#2215=EDGE_CURVE('',#1853,#1853,#1634,.T.);
#2216=EDGE_CURVE('',#1853,#1833,#1062,.T.);
#2217=EDGE_CURVE('',#1854,#1854,#1635,.T.);
#2218=EDGE_CURVE('',#1854,#1855,#1063,.T.);
#2219=EDGE_CURVE('',#1855,#1855,#1636,.T.);
#2220=EDGE_CURVE('',#1856,#1856,#1637,.T.);
#2221=EDGE_CURVE('',#1856,#1857,#1064,.T.);
#2222=EDGE_CURVE('',#1857,#1857,#1638,.T.);
#2223=EDGE_CURVE('',#1858,#1858,#1639,.T.);
#2224=EDGE_CURVE('',#1858,#1859,#1065,.T.);
#2225=EDGE_CURVE('',#1859,#1859,#1640,.T.);
#2226=EDGE_CURVE('',#1860,#1860,#1641,.T.);
#2227=EDGE_CURVE('',#1860,#1861,#1066,.T.);
#2228=EDGE_CURVE('',#1861,#1861,#1642,.T.);
#2229=EDGE_CURVE('',#1862,#1862,#1643,.T.);
#2230=EDGE_CURVE('',#1862,#1863,#1067,.T.);
#2231=EDGE_CURVE('',#1863,#1863,#1644,.T.);
#2232=EDGE_CURVE('',#1864,#1864,#1645,.T.);
#2233=EDGE_CURVE('',#1864,#1865,#1068,.T.);
#2234=EDGE_CURVE('',#1865,#1865,#1646,.T.);
#2235=EDGE_CURVE('',#1866,#1867,#1647,.T.);
#2236=EDGE_CURVE('',#1868,#1866,#1069,.T.);
#2237=EDGE_CURVE('',#1869,#1868,#1648,.T.);
#2238=EDGE_CURVE('',#1867,#1869,#1070,.T.);
#2239=EDGE_CURVE('',#1870,#1868,#1071,.T.);
#2240=EDGE_CURVE('',#1871,#1870,#1072,.T.);
#2241=EDGE_CURVE('',#1871,#1872,#1073,.T.);
#2242=EDGE_CURVE('',#1872,#1873,#1074,.T.);
#2243=EDGE_CURVE('',#1869,#1873,#1075,.T.);
#2244=EDGE_CURVE('',#1866,#1874,#1076,.T.);
#2245=EDGE_CURVE('',#1874,#1870,#1077,.T.);
#2246=EDGE_CURVE('',#1872,#1875,#1078,.T.);
#2247=EDGE_CURVE('',#1875,#1876,#1079,.T.);
#2248=EDGE_CURVE('',#1873,#1876,#1080,.T.);
#2249=EDGE_CURVE('',#1877,#1871,#1081,.T.);
#2250=EDGE_CURVE('',#1877,#1874,#1082,.T.);
#2251=EDGE_CURVE('',#1876,#1867,#1083,.T.);
#2252=EDGE_CURVE('',#1875,#1877,#1084,.T.);
#2253=EDGE_CURVE('',#1878,#1879,#1085,.T.);
#2254=EDGE_CURVE('',#1878,#1879,#1649,.T.);
#2255=EDGE_CURVE('',#1880,#1880,#1650,.T.);
#2256=EDGE_CURVE('',#1881,#1878,#1086,.T.);
#2257=EDGE_CURVE('',#1882,#1881,#1651,.T.);
#2258=EDGE_CURVE('',#1879,#1882,#1087,.T.);
#2259=EDGE_CURVE('',#1883,#1884,#1088,.T.);
#2260=EDGE_CURVE('',#1883,#1884,#1652,.T.);
#2261=EDGE_CURVE('',#1885,#1885,#1653,.T.);
#2262=EDGE_CURVE('',#1886,#1883,#1089,.T.);
#2263=EDGE_CURVE('',#1887,#1886,#1654,.T.);
#2264=EDGE_CURVE('',#1884,#1887,#1090,.T.);
#2265=EDGE_CURVE('',#1888,#1882,#1091,.T.);
#2266=EDGE_CURVE('',#1889,#1888,#1092,.T.);
#2267=EDGE_CURVE('',#1889,#1890,#1093,.T.);
#2268=EDGE_CURVE('',#1890,#1891,#1094,.T.);
#2269=EDGE_CURVE('',#1881,#1891,#1095,.T.);
#2270=EDGE_CURVE('',#1892,#1887,#1096,.T.);
#2271=EDGE_CURVE('',#1893,#1892,#1097,.T.);
#2272=EDGE_CURVE('',#1893,#1894,#1098,.T.);
#2273=EDGE_CURVE('',#1894,#1895,#1099,.T.);
#2274=EDGE_CURVE('',#1886,#1895,#1100,.T.);
#2275=EDGE_CURVE('',#1896,#1896,#1655,.T.);
#2276=EDGE_CURVE('',#1896,#1880,#1101,.T.);
#2277=EDGE_CURVE('',#1897,#1897,#1656,.T.);
#2278=EDGE_CURVE('',#1897,#1885,#1102,.T.);
#2279=EDGE_CURVE('',#1898,#1899,#1657,.T.);
#2280=EDGE_CURVE('',#1900,#1898,#1103,.T.);
#2281=EDGE_CURVE('',#1901,#1900,#1658,.T.);
#2282=EDGE_CURVE('',#1899,#1901,#1104,.T.);
#2283=EDGE_CURVE('',#1900,#1893,#1105,.T.);
#2284=EDGE_CURVE('',#1891,#1892,#1106,.T.);
#2285=EDGE_CURVE('',#1890,#1901,#1107,.T.);
#2286=EDGE_CURVE('',#1894,#1898,#1108,.T.);
#2287=EDGE_CURVE('',#1899,#1889,#1109,.T.);
#2288=EDGE_CURVE('',#1895,#1888,#1110,.T.);
#2289=EDGE_CURVE('',#1902,#1902,#1659,.T.);
#2290=EDGE_CURVE('',#1902,#1903,#1111,.T.);
#2291=EDGE_CURVE('',#1903,#1903,#1660,.T.);
#2292=EDGE_CURVE('',#1904,#1904,#1661,.T.);
#2293=EDGE_CURVE('',#1904,#1905,#1112,.T.);
#2294=EDGE_CURVE('',#1905,#1905,#1662,.T.);
#2295=EDGE_CURVE('',#1906,#1906,#1663,.T.);
#2296=EDGE_CURVE('',#1906,#1907,#1113,.T.);
#2297=EDGE_CURVE('',#1907,#1907,#1664,.T.);
#2298=EDGE_CURVE('',#1908,#1908,#1665,.T.);
#2299=EDGE_CURVE('',#1908,#1909,#1114,.T.);
#2300=EDGE_CURVE('',#1909,#1909,#1666,.T.);
#2301=EDGE_CURVE('',#1910,#1911,#1667,.T.);
#2302=EDGE_CURVE('',#1912,#1910,#1115,.T.);
#2303=EDGE_CURVE('',#1913,#1912,#1668,.T.);
#2304=EDGE_CURVE('',#1911,#1913,#1116,.T.);
#2305=EDGE_CURVE('',#1914,#1912,#1117,.T.);
#2306=EDGE_CURVE('',#1915,#1914,#1118,.T.);
#2307=EDGE_CURVE('',#1915,#1916,#1119,.T.);
#2308=EDGE_CURVE('',#1916,#1917,#1120,.T.);
#2309=EDGE_CURVE('',#1913,#1917,#1121,.T.);
#2310=EDGE_CURVE('',#1910,#1918,#1122,.T.);
#2311=EDGE_CURVE('',#1918,#1914,#1123,.T.);
#2312=EDGE_CURVE('',#1916,#1919,#1124,.T.);
#2313=EDGE_CURVE('',#1919,#1920,#1125,.T.);
#2314=EDGE_CURVE('',#1917,#1920,#1126,.T.);
#2315=EDGE_CURVE('',#1921,#1915,#1127,.T.);
#2316=EDGE_CURVE('',#1921,#1918,#1128,.T.);
#2317=EDGE_CURVE('',#1920,#1911,#1129,.T.);
#2318=EDGE_CURVE('',#1919,#1921,#1130,.T.);
#2319=EDGE_CURVE('',#1922,#1923,#1131,.T.);
#2320=EDGE_CURVE('',#1922,#1923,#1669,.T.);
#2321=EDGE_CURVE('',#1924,#1924,#1670,.T.);
#2322=EDGE_CURVE('',#1925,#1922,#1132,.T.);
#2323=EDGE_CURVE('',#1926,#1925,#1671,.T.);
#2324=EDGE_CURVE('',#1923,#1926,#1133,.T.);
#2325=EDGE_CURVE('',#1927,#1928,#1134,.T.);
#2326=EDGE_CURVE('',#1927,#1928,#1672,.T.);
#2327=EDGE_CURVE('',#1929,#1929,#1673,.T.);
#2328=EDGE_CURVE('',#1930,#1927,#1135,.T.);
#2329=EDGE_CURVE('',#1931,#1930,#1674,.T.);
#2330=EDGE_CURVE('',#1928,#1931,#1136,.T.);
#2331=EDGE_CURVE('',#1932,#1926,#1137,.T.);
#2332=EDGE_CURVE('',#1933,#1932,#1138,.T.);
#2333=EDGE_CURVE('',#1933,#1934,#1139,.T.);
#2334=EDGE_CURVE('',#1934,#1935,#1140,.T.);
#2335=EDGE_CURVE('',#1925,#1935,#1141,.T.);
#2336=EDGE_CURVE('',#1936,#1931,#1142,.T.);
#2337=EDGE_CURVE('',#1937,#1936,#1143,.T.);
#2338=EDGE_CURVE('',#1937,#1938,#1144,.T.);
#2339=EDGE_CURVE('',#1938,#1939,#1145,.T.);
#2340=EDGE_CURVE('',#1930,#1939,#1146,.T.);
#2341=EDGE_CURVE('',#1940,#1940,#1675,.T.);
#2342=EDGE_CURVE('',#1940,#1924,#1147,.T.);
#2343=EDGE_CURVE('',#1941,#1941,#1676,.T.);
#2344=EDGE_CURVE('',#1941,#1929,#1148,.T.);
#2345=EDGE_CURVE('',#1942,#1943,#1677,.T.);
#2346=EDGE_CURVE('',#1944,#1942,#1149,.T.);
#2347=EDGE_CURVE('',#1945,#1944,#1678,.T.);
#2348=EDGE_CURVE('',#1943,#1945,#1150,.T.);
#2349=EDGE_CURVE('',#1944,#1937,#1151,.T.);
#2350=EDGE_CURVE('',#1935,#1936,#1152,.T.);
#2351=EDGE_CURVE('',#1934,#1945,#1153,.T.);
#2352=EDGE_CURVE('',#1938,#1942,#1154,.T.);
#2353=EDGE_CURVE('',#1943,#1933,#1155,.T.);
#2354=EDGE_CURVE('',#1939,#1932,#1156,.T.);
#2355=EDGE_CURVE('',#1946,#1946,#1679,.T.);
#2356=EDGE_CURVE('',#1946,#1947,#1157,.T.);
#2357=EDGE_CURVE('',#1947,#1947,#1680,.T.);
#2358=EDGE_CURVE('',#1948,#1948,#1681,.T.);
#2359=EDGE_CURVE('',#1948,#1949,#1158,.T.);
#2360=EDGE_CURVE('',#1949,#1949,#1682,.T.);
#2361=EDGE_CURVE('',#1950,#1950,#1683,.T.);
#2362=EDGE_CURVE('',#1950,#1951,#1159,.T.);
#2363=EDGE_CURVE('',#1951,#1951,#1684,.T.);
#2364=EDGE_CURVE('',#1952,#1952,#1685,.T.);
#2365=EDGE_CURVE('',#1952,#1953,#1160,.T.);
#2366=EDGE_CURVE('',#1953,#1953,#1686,.T.);
#2367=EDGE_CURVE('',#1954,#1954,#1687,.T.);
#2368=EDGE_CURVE('',#1954,#1955,#1161,.T.);
#2369=EDGE_CURVE('',#1955,#1955,#1688,.T.);
#2370=EDGE_CURVE('',#1956,#1956,#1689,.T.);
#2371=EDGE_CURVE('',#1956,#1957,#1162,.T.);
#2372=EDGE_CURVE('',#1957,#1957,#1690,.T.);
#2373=EDGE_CURVE('',#1958,#1958,#1691,.T.);
#2374=EDGE_CURVE('',#1958,#1959,#1163,.T.);
#2375=EDGE_CURVE('',#1959,#1959,#1692,.T.);
#2376=EDGE_CURVE('',#1960,#1960,#1693,.T.);
#2377=EDGE_CURVE('',#1960,#1961,#1164,.T.);
#2378=EDGE_CURVE('',#1961,#1961,#1694,.T.);
#2379=EDGE_CURVE('',#1962,#1962,#1695,.T.);
#2380=EDGE_CURVE('',#1962,#1963,#1165,.T.);
#2381=EDGE_CURVE('',#1963,#1963,#1696,.T.);
#2382=EDGE_CURVE('',#1964,#1964,#1697,.T.);
#2383=EDGE_CURVE('',#1964,#1965,#1166,.T.);
#2384=EDGE_CURVE('',#1965,#1965,#1698,.T.);
#2385=EDGE_CURVE('',#1966,#1966,#1699,.T.);
#2386=EDGE_CURVE('',#1967,#1967,#1700,.T.);
#2387=EDGE_CURVE('',#1967,#1966,#1167,.T.);
#2388=EDGE_CURVE('',#1968,#1968,#1701,.T.);
#2389=EDGE_CURVE('',#1968,#1969,#1168,.T.);
#2390=EDGE_CURVE('',#1969,#1969,#1702,.T.);
#2391=EDGE_CURVE('',#1970,#1971,#1169,.T.);
#2392=EDGE_CURVE('',#1971,#1970,#1703,.T.);
#2393=EDGE_CURVE('',#1972,#1972,#1704,.T.);
#2394=EDGE_CURVE('',#1972,#1973,#1170,.T.);
#2395=EDGE_CURVE('',#1971,#1973,#183,.T.);
#2396=EDGE_CURVE('',#1973,#1970,#184,.T.);
#2397=EDGE_CURVE('',#1974,#1975,#185,.T.);
#2398=EDGE_CURVE('',#1975,#1974,#186,.T.);
#2399=EDGE_CURVE('',#1975,#1976,#1171,.T.);
#2400=EDGE_CURVE('',#1976,#1976,#1705,.T.);
#2401=EDGE_CURVE('',#1977,#1978,#1706,.T.);
#2402=EDGE_CURVE('',#1978,#1977,#1707,.T.);
#2403=EDGE_CURVE('',#1979,#1979,#1708,.T.);
#2404=EDGE_CURVE('',#1979,#1980,#1172,.T.);
#2405=EDGE_CURVE('',#1981,#1980,#1709,.T.);
#2406=EDGE_CURVE('',#1978,#1981,#1173,.T.);
#2407=EDGE_CURVE('',#1982,#1977,#1174,.T.);
#2408=EDGE_CURVE('',#1980,#1982,#1710,.T.);
#2409=EDGE_CURVE('',#1983,#1984,#1711,.T.);
#2410=EDGE_CURVE('',#1984,#1983,#1712,.T.);
#2411=EDGE_CURVE('',#1985,#1985,#1713,.T.);
#2412=EDGE_CURVE('',#1985,#1986,#1175,.T.);
#2413=EDGE_CURVE('',#1987,#1986,#1714,.T.);
#2414=EDGE_CURVE('',#1984,#1987,#1176,.T.);
#2415=EDGE_CURVE('',#1988,#1983,#1177,.T.);
#2416=EDGE_CURVE('',#1986,#1988,#1715,.T.);
#2417=EDGE_CURVE('',#1989,#1990,#1716,.T.);
#2418=EDGE_CURVE('',#1990,#1989,#1717,.T.);
#2419=EDGE_CURVE('',#1991,#1991,#1718,.T.);
#2420=EDGE_CURVE('',#1991,#1992,#1178,.T.);
#2421=EDGE_CURVE('',#1993,#1992,#1719,.T.);
#2422=EDGE_CURVE('',#1990,#1993,#1179,.T.);
#2423=EDGE_CURVE('',#1994,#1989,#1180,.T.);
#2424=EDGE_CURVE('',#1992,#1994,#1720,.T.);
#2425=EDGE_CURVE('',#1988,#1981,#1721,.T.);
#2426=EDGE_CURVE('',#1994,#1987,#1722,.T.);
#2427=EDGE_CURVE('',#1995,#1993,#1723,.T.);
#2428=EDGE_CURVE('',#1995,#1996,#1181,.T.);
#2429=EDGE_CURVE('',#1997,#1996,#1724,.T.);
#2430=EDGE_CURVE('',#1997,#1998,#1182,.T.);
#2431=EDGE_CURVE('',#1982,#1998,#1725,.T.);
#2432=EDGE_CURVE('',#1999,#2000,#1183,.T.);
#2433=EDGE_CURVE('',#1998,#1999,#1184,.T.);
#2434=EDGE_CURVE('',#2000,#1997,#1185,.T.);
#2435=EDGE_CURVE('',#2001,#2002,#1186,.T.);
#2436=EDGE_CURVE('',#1996,#2001,#1187,.T.);
#2437=EDGE_CURVE('',#2002,#1995,#1188,.T.);
#2438=EDGE_CURVE('',#2003,#2003,#1726,.T.);
#2439=EDGE_CURVE('',#2002,#1999,#1727,.T.);
#2440=EDGE_CURVE('',#2001,#2004,#1728,.T.);
#2441=EDGE_CURVE('',#2004,#2000,#1729,.T.);
#2442=EDGE_CURVE('',#2004,#2005,#1189,.T.);
#2443=EDGE_CURVE('',#2005,#2005,#1730,.T.);
#2444=EDGE_CURVE('',#2003,#2006,#1190,.T.);
#2445=EDGE_CURVE('',#2006,#2006,#1731,.T.);
#2446=EDGE_CURVE('',#2007,#2007,#1732,.T.);
#2447=EDGE_CURVE('',#2008,#2008,#1733,.T.);
#2448=EDGE_CURVE('',#2008,#2007,#1191,.T.);
#2449=EDGE_CURVE('',#2009,#2009,#1734,.T.);
#2450=EDGE_CURVE('',#2009,#2008,#1192,.T.);
#2451=EDGE_CURVE('',#2010,#2010,#1735,.T.);
#2452=EDGE_CURVE('',#2010,#2009,#1193,.T.);
#2453=EDGE_CURVE('',#2011,#2011,#1736,.T.);
#2454=EDGE_CURVE('',#2012,#2012,#1737,.F.);
#2455=EDGE_CURVE('',#2012,#2011,#1194,.T.);
#2456=EDGE_CURVE('',#2013,#2013,#1738,.F.);
#2457=EDGE_CURVE('',#2013,#2012,#1195,.T.);
#2458=EDGE_CURVE('',#2014,#2014,#1739,.T.);
#2459=EDGE_CURVE('',#2014,#2013,#1196,.T.);
#2460=EDGE_CURVE('',#2015,#2016,#1197,.T.);
#2461=EDGE_CURVE('',#2016,#2017,#1198,.T.);
#2462=EDGE_CURVE('',#2017,#2018,#1199,.T.);
#2463=EDGE_CURVE('',#2015,#2018,#1200,.T.);
#2464=EDGE_CURVE('',#2016,#2019,#1201,.T.);
#2465=EDGE_CURVE('',#2019,#2020,#1202,.T.);
#2466=EDGE_CURVE('',#2020,#2017,#1203,.T.);
#2467=EDGE_CURVE('',#2019,#2021,#1204,.T.);
#2468=EDGE_CURVE('',#2021,#2022,#1205,.T.);
#2469=EDGE_CURVE('',#2022,#2020,#1206,.T.);
#2470=EDGE_CURVE('',#2021,#2023,#1207,.T.);
#2471=EDGE_CURVE('',#2023,#2024,#1208,.T.);
#2472=EDGE_CURVE('',#2024,#2022,#1209,.T.);
#2473=EDGE_CURVE('',#2023,#2025,#1210,.T.);
#2474=EDGE_CURVE('',#2025,#2026,#1211,.T.);
#2475=EDGE_CURVE('',#2026,#2024,#1212,.T.);
#2476=EDGE_CURVE('',#2025,#2015,#1213,.T.);
#2477=EDGE_CURVE('',#2018,#2026,#1214,.T.);
#2478=EDGE_CURVE('',#2027,#2028,#1740,.T.);
#2479=EDGE_CURVE('',#2029,#2027,#1215,.T.);
#2480=EDGE_CURVE('',#2030,#2029,#1216,.T.);
#2481=EDGE_CURVE('',#2028,#2030,#1217,.T.);
#2482=EDGE_CURVE('',#2028,#2031,#1218,.T.);
#2483=EDGE_CURVE('',#2032,#2030,#1219,.T.);
#2484=EDGE_CURVE('',#2032,#2031,#1220,.T.);
#2485=EDGE_CURVE('',#2031,#2033,#1741,.T.);
#2486=EDGE_CURVE('',#2034,#2032,#1221,.T.);
#2487=EDGE_CURVE('',#2033,#2034,#1222,.T.);
#2488=EDGE_CURVE('',#2033,#2027,#1223,.T.);
#2489=EDGE_CURVE('',#2034,#2029,#1224,.T.);
#2490=EDGE_CURVE('',#2035,#2035,#1742,.T.);
#2491=EDGE_CURVE('',#2036,#2036,#1743,.T.);
#2492=EDGE_CURVE('',#2037,#2037,#1744,.T.);
#2493=EDGE_CURVE('',#2037,#2035,#1225,.T.);
#2494=EDGE_CURVE('',#2038,#2038,#1745,.T.);
#2495=EDGE_CURVE('',#2039,#2039,#1746,.T.);
#2496=EDGE_CURVE('',#2039,#2038,#1226,.T.);
#2497=EDGE_CURVE('',#2040,#2040,#1747,.T.);
#2498=EDGE_CURVE('',#2041,#2041,#1748,.T.);
#2499=EDGE_CURVE('',#2041,#2040,#1227,.T.);
#2500=EDGE_CURVE('',#2042,#2042,#1749,.T.);
#2501=EDGE_CURVE('',#2043,#2043,#1750,.T.);
#2502=EDGE_CURVE('',#2043,#2042,#1228,.T.);
#2503=EDGE_CURVE('',#2044,#2044,#1751,.T.);
#2504=EDGE_CURVE('',#2045,#2045,#1752,.T.);
#2505=EDGE_CURVE('',#2045,#2044,#1229,.T.);
#2506=EDGE_CURVE('',#2046,#2046,#1753,.T.);
#2507=EDGE_CURVE('',#2046,#2036,#1230,.T.);
#2508=EDGE_CURVE('',#2047,#2048,#1754,.T.);
#2509=EDGE_CURVE('',#2049,#2047,#1231,.T.);
#2510=EDGE_CURVE('',#2050,#2049,#1755,.T.);
#2511=EDGE_CURVE('',#2048,#2050,#1232,.T.);
#2512=EDGE_CURVE('',#2048,#2051,#1233,.T.);
#2513=EDGE_CURVE('',#2052,#2050,#1234,.T.);
#2514=EDGE_CURVE('',#2052,#2051,#1235,.T.);
#2515=EDGE_CURVE('',#2051,#2053,#1756,.T.);
#2516=EDGE_CURVE('',#2054,#2052,#1757,.T.);
#2517=EDGE_CURVE('',#2053,#2054,#1236,.T.);
#2518=EDGE_CURVE('',#2053,#2047,#1237,.T.);
#2519=EDGE_CURVE('',#2049,#2054,#1238,.T.);
#2520=EDGE_CURVE('',#2055,#2055,#1758,.T.);
#2521=EDGE_CURVE('',#2056,#2056,#1759,.T.);
#2522=EDGE_CURVE('',#2057,#2057,#1760,.T.);
#2523=EDGE_CURVE('',#2057,#2055,#1239,.T.);
#2524=EDGE_CURVE('',#2058,#2058,#1761,.T.);
#2525=EDGE_CURVE('',#2058,#2056,#1240,.T.);
#2526=EDGE_CURVE('',#2059,#2060,#1241,.T.);
#2527=EDGE_CURVE('',#2059,#2060,#1762,.T.);
#2528=EDGE_CURVE('',#2061,#2062,#187,.T.);
#2529=EDGE_CURVE('',#2063,#2061,#1763,.T.);
#2530=EDGE_CURVE('',#2064,#2063,#188,.T.);
#2531=EDGE_CURVE('',#2060,#2064,#189,.T.);
#2532=EDGE_CURVE('',#2062,#2059,#190,.T.);
#2533=EDGE_CURVE('',#2062,#2065,#1242,.T.);
#2534=EDGE_CURVE('',#2066,#2065,#191,.T.);
#2535=EDGE_CURVE('',#2067,#2066,#192,.T.);
#2536=EDGE_CURVE('',#2065,#2067,#193,.T.);
#2537=EDGE_CURVE('',#2063,#2061,#1243,.T.);
#2538=EDGE_CURVE('',#2068,#2068,#1764,.T.);
#2539=EDGE_CURVE('',#2068,#2064,#1244,.T.);
#2540=EDGE_CURVE('',#2062,#2069,#1245,.T.);
#2541=EDGE_CURVE('',#2069,#2069,#1765,.T.);
#2542=EDGE_CURVE('',#2070,#2070,#1766,.T.);
#2543=EDGE_CURVE('',#2070,#2067,#1246,.T.);
#2544=EDGE_CURVE('',#2065,#2071,#1247,.T.);
#2545=EDGE_CURVE('',#2071,#2071,#1767,.T.);
#2546=EDGE_CURVE('',#2072,#2073,#1248,.T.);
#2547=EDGE_CURVE('',#2072,#2073,#1768,.T.);
#2548=EDGE_CURVE('',#2074,#2075,#194,.T.);
#2549=EDGE_CURVE('',#2076,#2074,#1769,.T.);
#2550=EDGE_CURVE('',#2077,#2076,#195,.T.);
#2551=EDGE_CURVE('',#2073,#2077,#196,.T.);
#2552=EDGE_CURVE('',#2075,#2072,#197,.T.);
#2553=EDGE_CURVE('',#2075,#2078,#1249,.T.);
#2554=EDGE_CURVE('',#2079,#2078,#198,.T.);
#2555=EDGE_CURVE('',#2080,#2079,#199,.T.);
#2556=EDGE_CURVE('',#2078,#2080,#200,.T.);
#2557=EDGE_CURVE('',#2076,#2074,#1250,.T.);
#2558=EDGE_CURVE('',#2081,#2081,#1770,.T.);
#2559=EDGE_CURVE('',#2081,#2077,#1251,.T.);
#2560=EDGE_CURVE('',#2075,#2082,#1252,.T.);
#2561=EDGE_CURVE('',#2082,#2082,#1771,.T.);
#2562=EDGE_CURVE('',#2083,#2083,#1772,.T.);
#2563=EDGE_CURVE('',#2083,#2080,#1253,.T.);
#2564=EDGE_CURVE('',#2078,#2084,#1254,.T.);
#2565=EDGE_CURVE('',#2084,#2084,#1773,.T.);
#2566=EDGE_CURVE('',#2085,#2085,#1774,.T.);
#2567=EDGE_CURVE('',#2085,#2086,#1255,.T.);
#2568=EDGE_CURVE('',#2086,#2086,#1775,.T.);
#2569=EDGE_CURVE('',#2087,#2087,#1776,.T.);
#2570=EDGE_CURVE('',#2087,#2088,#1256,.T.);
#2571=EDGE_CURVE('',#2088,#2088,#1777,.T.);
#2572=EDGE_CURVE('',#2089,#2089,#1778,.T.);
#2573=EDGE_CURVE('',#2089,#2090,#1257,.T.);
#2574=EDGE_CURVE('',#2090,#2090,#1779,.T.);
#2575=EDGE_CURVE('',#2091,#2091,#1780,.T.);
#2576=EDGE_CURVE('',#2091,#2092,#1258,.T.);
#2577=EDGE_CURVE('',#2092,#2092,#1781,.T.);
#2578=EDGE_CURVE('',#2093,#2093,#1782,.T.);
#2579=EDGE_CURVE('',#2093,#2094,#1259,.T.);
#2580=EDGE_CURVE('',#2094,#2094,#1783,.T.);
#2581=EDGE_CURVE('',#2095,#2095,#1784,.T.);
#2582=EDGE_CURVE('',#2095,#2093,#1260,.T.);
#2583=EDGE_CURVE('',#2096,#2096,#1785,.T.);
#2584=EDGE_CURVE('',#2096,#2095,#1261,.T.);
#2585=EDGE_CURVE('',#2097,#2098,#1262,.T.);
#2586=EDGE_CURVE('',#2097,#2099,#1263,.T.);
#2587=EDGE_CURVE('',#2099,#2100,#1264,.T.);
#2588=EDGE_CURVE('',#2098,#2100,#1265,.T.);
#2589=EDGE_CURVE('',#2101,#2097,#1266,.T.);
#2590=EDGE_CURVE('',#2101,#2102,#1267,.T.);
#2591=EDGE_CURVE('',#2102,#2099,#1268,.T.);
#2592=EDGE_CURVE('',#2103,#2101,#1269,.T.);
#2593=EDGE_CURVE('',#2103,#2104,#1270,.T.);
#2594=EDGE_CURVE('',#2104,#2102,#1271,.T.);
#2595=EDGE_CURVE('',#2105,#2103,#1272,.T.);
#2596=EDGE_CURVE('',#2105,#2106,#1273,.T.);
#2597=EDGE_CURVE('',#2106,#2104,#1274,.T.);
#2598=EDGE_CURVE('',#2107,#2105,#1275,.T.);
#2599=EDGE_CURVE('',#2107,#2108,#1276,.T.);
#2600=EDGE_CURVE('',#2108,#2106,#1277,.T.);
#2601=EDGE_CURVE('',#2098,#2107,#1278,.T.);
#2602=EDGE_CURVE('',#2100,#2108,#1279,.T.);
#2603=EDGE_CURVE('',#2109,#2109,#1786,.T.);
#2604=EDGE_CURVE('',#2110,#2110,#1787,.T.);
#2605=EDGE_CURVE('',#2110,#2109,#1280,.T.);
#2606=EDGE_CURVE('',#2111,#2111,#1788,.F.);
#2607=EDGE_CURVE('',#2111,#2110,#1281,.T.);
#2608=EDGE_CURVE('',#2112,#2112,#1789,.T.);
#2609=EDGE_CURVE('',#2112,#2111,#1282,.T.);
#2610=EDGE_CURVE('',#2113,#2113,#1790,.T.);
#2611=EDGE_CURVE('',#2114,#2114,#1791,.T.);
#2612=EDGE_CURVE('',#2114,#2113,#1283,.T.);
#2613=EDGE_CURVE('',#2115,#2115,#1792,.T.);
#2614=EDGE_CURVE('',#2115,#2114,#1284,.T.);
#2615=EDGE_CURVE('',#2116,#2116,#1793,.T.);
#2616=EDGE_CURVE('',#2116,#2115,#1285,.T.);
#2617=EDGE_CURVE('',#2117,#2117,#1794,.T.);
#2618=EDGE_CURVE('',#2118,#2118,#1795,.F.);
#2619=EDGE_CURVE('',#2118,#2117,#1286,.T.);
#2620=EDGE_CURVE('',#2119,#2119,#1796,.F.);
#2621=EDGE_CURVE('',#2119,#2118,#1287,.T.);
#2622=EDGE_CURVE('',#2120,#2120,#1797,.T.);
#2623=EDGE_CURVE('',#2120,#2119,#1288,.T.);
#2624=EDGE_CURVE('',#2121,#2122,#1289,.T.);
#2625=EDGE_CURVE('',#2122,#2123,#1290,.T.);
#2626=EDGE_CURVE('',#2123,#2124,#1291,.T.);
#2627=EDGE_CURVE('',#2121,#2124,#1292,.T.);
#2628=EDGE_CURVE('',#2122,#2125,#1293,.T.);
#2629=EDGE_CURVE('',#2125,#2126,#1294,.T.);
#2630=EDGE_CURVE('',#2126,#2123,#1295,.T.);
#2631=EDGE_CURVE('',#2125,#2127,#1296,.T.);
#2632=EDGE_CURVE('',#2127,#2128,#1297,.T.);
#2633=EDGE_CURVE('',#2128,#2126,#1298,.T.);
#2634=EDGE_CURVE('',#2127,#2129,#1299,.T.);
#2635=EDGE_CURVE('',#2129,#2130,#1300,.T.);
#2636=EDGE_CURVE('',#2130,#2128,#1301,.T.);
#2637=EDGE_CURVE('',#2129,#2131,#1302,.T.);
#2638=EDGE_CURVE('',#2131,#2132,#1303,.T.);
#2639=EDGE_CURVE('',#2132,#2130,#1304,.T.);
#2640=EDGE_CURVE('',#2131,#2121,#1305,.T.);
#2641=EDGE_CURVE('',#2124,#2132,#1306,.T.);
#2642=ORIENTED_EDGE('',*,*,#2133,.F.);
#2643=ORIENTED_EDGE('',*,*,#2134,.T.);
#2644=ORIENTED_EDGE('',*,*,#2135,.F.);
#2645=ORIENTED_EDGE('',*,*,#2134,.F.);
#2646=ORIENTED_EDGE('',*,*,#2136,.F.);
#2647=ORIENTED_EDGE('',*,*,#2137,.T.);
#2648=ORIENTED_EDGE('',*,*,#2138,.F.);
#2649=ORIENTED_EDGE('',*,*,#2137,.F.);
#2650=ORIENTED_EDGE('',*,*,#2139,.F.);
#2651=ORIENTED_EDGE('',*,*,#2140,.T.);
#2652=ORIENTED_EDGE('',*,*,#2141,.F.);
#2653=ORIENTED_EDGE('',*,*,#2140,.F.);
#2654=ORIENTED_EDGE('',*,*,#2142,.F.);
#2655=ORIENTED_EDGE('',*,*,#2143,.T.);
#2656=ORIENTED_EDGE('',*,*,#2144,.F.);
#2657=ORIENTED_EDGE('',*,*,#2143,.F.);
#2658=ORIENTED_EDGE('',*,*,#2145,.T.);
#2659=ORIENTED_EDGE('',*,*,#2146,.T.);
#2660=ORIENTED_EDGE('',*,*,#2147,.F.);
#2661=ORIENTED_EDGE('',*,*,#2148,.F.);
#2662=ORIENTED_EDGE('',*,*,#2149,.T.);
#2663=ORIENTED_EDGE('',*,*,#2148,.T.);
#2664=ORIENTED_EDGE('',*,*,#2150,.F.);
#2665=ORIENTED_EDGE('',*,*,#2151,.F.);
#2666=ORIENTED_EDGE('',*,*,#2152,.T.);
#2667=ORIENTED_EDGE('',*,*,#2151,.T.);
#2668=ORIENTED_EDGE('',*,*,#2153,.F.);
#2669=ORIENTED_EDGE('',*,*,#2154,.F.);
#2670=ORIENTED_EDGE('',*,*,#2155,.T.);
#2671=ORIENTED_EDGE('',*,*,#2154,.T.);
#2672=ORIENTED_EDGE('',*,*,#2156,.F.);
#2673=ORIENTED_EDGE('',*,*,#2146,.F.);
#2674=ORIENTED_EDGE('',*,*,#2156,.T.);
#2675=ORIENTED_EDGE('',*,*,#2153,.T.);
#2676=ORIENTED_EDGE('',*,*,#2150,.T.);
#2677=ORIENTED_EDGE('',*,*,#2147,.T.);
#2678=ORIENTED_EDGE('',*,*,#2135,.T.);
#2679=ORIENTED_EDGE('',*,*,#2138,.T.);
#2680=ORIENTED_EDGE('',*,*,#2141,.T.);
#2681=ORIENTED_EDGE('',*,*,#2144,.T.);
#2682=ORIENTED_EDGE('',*,*,#2155,.F.);
#2683=ORIENTED_EDGE('',*,*,#2145,.F.);
#2684=ORIENTED_EDGE('',*,*,#2149,.F.);
#2685=ORIENTED_EDGE('',*,*,#2152,.F.);
#2686=ORIENTED_EDGE('',*,*,#2133,.T.);
#2687=ORIENTED_EDGE('',*,*,#2136,.T.);
#2688=ORIENTED_EDGE('',*,*,#2139,.T.);
#2689=ORIENTED_EDGE('',*,*,#2142,.T.);
#2690=ORIENTED_EDGE('',*,*,#2157,.F.);
#2691=ORIENTED_EDGE('',*,*,#2158,.F.);
#2692=ORIENTED_EDGE('',*,*,#2159,.F.);
#2693=ORIENTED_EDGE('',*,*,#2160,.F.);
#2694=ORIENTED_EDGE('',*,*,#2161,.T.);
#2695=ORIENTED_EDGE('',*,*,#2162,.F.);
#2696=ORIENTED_EDGE('',*,*,#2161,.F.);
#2697=ORIENTED_EDGE('',*,*,#2163,.F.);
#2698=ORIENTED_EDGE('',*,*,#2164,.F.);
#2699=ORIENTED_EDGE('',*,*,#2158,.T.);
#2700=ORIENTED_EDGE('',*,*,#2165,.F.);
#2701=ORIENTED_EDGE('',*,*,#2166,.F.);
#2702=ORIENTED_EDGE('',*,*,#2167,.F.);
#2703=ORIENTED_EDGE('',*,*,#2168,.F.);
#2704=ORIENTED_EDGE('',*,*,#2169,.F.);
#2705=ORIENTED_EDGE('',*,*,#2170,.T.);
#2706=ORIENTED_EDGE('',*,*,#2171,.F.);
#2707=ORIENTED_EDGE('',*,*,#2170,.F.);
#2708=ORIENTED_EDGE('',*,*,#2172,.F.);
#2709=ORIENTED_EDGE('',*,*,#2173,.F.);
#2710=ORIENTED_EDGE('',*,*,#2167,.T.);
#2711=ORIENTED_EDGE('',*,*,#2174,.F.);
#2712=ORIENTED_EDGE('',*,*,#2175,.F.);
#2713=ORIENTED_EDGE('',*,*,#2176,.F.);
#2714=ORIENTED_EDGE('',*,*,#2177,.F.);
#2715=ORIENTED_EDGE('',*,*,#2178,.T.);
#2716=ORIENTED_EDGE('',*,*,#2179,.F.);
#2717=ORIENTED_EDGE('',*,*,#2178,.F.);
#2718=ORIENTED_EDGE('',*,*,#2180,.F.);
#2719=ORIENTED_EDGE('',*,*,#2181,.F.);
#2720=ORIENTED_EDGE('',*,*,#2175,.T.);
#2721=ORIENTED_EDGE('',*,*,#2182,.F.);
#2722=ORIENTED_EDGE('',*,*,#2163,.T.);
#2723=ORIENTED_EDGE('',*,*,#2160,.T.);
#2724=ORIENTED_EDGE('',*,*,#2183,.F.);
#2725=ORIENTED_EDGE('',*,*,#2172,.T.);
#2726=ORIENTED_EDGE('',*,*,#2169,.T.);
#2727=ORIENTED_EDGE('',*,*,#2184,.F.);
#2728=ORIENTED_EDGE('',*,*,#2180,.T.);
#2729=ORIENTED_EDGE('',*,*,#2177,.T.);
#2730=ORIENTED_EDGE('',*,*,#2185,.F.);
#2731=ORIENTED_EDGE('',*,*,#2186,.F.);
#2732=ORIENTED_EDGE('',*,*,#2187,.F.);
#2733=ORIENTED_EDGE('',*,*,#2188,.F.);
#2734=ORIENTED_EDGE('',*,*,#2189,.F.);
#2735=ORIENTED_EDGE('',*,*,#2190,.T.);
#2736=ORIENTED_EDGE('',*,*,#2191,.F.);
#2737=ORIENTED_EDGE('',*,*,#2192,.F.);
#2738=ORIENTED_EDGE('',*,*,#2187,.T.);
#2739=ORIENTED_EDGE('',*,*,#2193,.F.);
#2740=ORIENTED_EDGE('',*,*,#2194,.F.);
#2741=ORIENTED_EDGE('',*,*,#2190,.F.);
#2742=ORIENTED_EDGE('',*,*,#2195,.F.);
#2743=ORIENTED_EDGE('',*,*,#2196,.F.);
#2744=ORIENTED_EDGE('',*,*,#2197,.F.);
#2745=ORIENTED_EDGE('',*,*,#2198,.T.);
#2746=ORIENTED_EDGE('',*,*,#2199,.F.);
#2747=ORIENTED_EDGE('',*,*,#2200,.F.);
#2748=ORIENTED_EDGE('',*,*,#2196,.T.);
#2749=ORIENTED_EDGE('',*,*,#2201,.F.);
#2750=ORIENTED_EDGE('',*,*,#2202,.F.);
#2751=ORIENTED_EDGE('',*,*,#2198,.F.);
#2752=ORIENTED_EDGE('',*,*,#2203,.F.);
#2753=ORIENTED_EDGE('',*,*,#2204,.F.);
#2754=ORIENTED_EDGE('',*,*,#2205,.F.);
#2755=ORIENTED_EDGE('',*,*,#2206,.T.);
#2756=ORIENTED_EDGE('',*,*,#2207,.F.);
#2757=ORIENTED_EDGE('',*,*,#2208,.F.);
#2758=ORIENTED_EDGE('',*,*,#2204,.T.);
#2759=ORIENTED_EDGE('',*,*,#2209,.F.);
#2760=ORIENTED_EDGE('',*,*,#2210,.F.);
#2761=ORIENTED_EDGE('',*,*,#2206,.F.);
#2762=ORIENTED_EDGE('',*,*,#2157,.T.);
#2763=ORIENTED_EDGE('',*,*,#2185,.T.);
#2764=ORIENTED_EDGE('',*,*,#2176,.T.);
#2765=ORIENTED_EDGE('',*,*,#2181,.T.);
#2766=ORIENTED_EDGE('',*,*,#2174,.T.);
#2767=ORIENTED_EDGE('',*,*,#2184,.T.);
#2768=ORIENTED_EDGE('',*,*,#2168,.T.);
#2769=ORIENTED_EDGE('',*,*,#2173,.T.);
#2770=ORIENTED_EDGE('',*,*,#2166,.T.);
#2771=ORIENTED_EDGE('',*,*,#2183,.T.);
#2772=ORIENTED_EDGE('',*,*,#2159,.T.);
#2773=ORIENTED_EDGE('',*,*,#2164,.T.);
#2774=ORIENTED_EDGE('',*,*,#2211,.T.);
#2775=ORIENTED_EDGE('',*,*,#2188,.T.);
#2776=ORIENTED_EDGE('',*,*,#2192,.T.);
#2777=ORIENTED_EDGE('',*,*,#2212,.T.);
#2778=ORIENTED_EDGE('',*,*,#2201,.T.);
#2779=ORIENTED_EDGE('',*,*,#2195,.T.);
#2780=ORIENTED_EDGE('',*,*,#2200,.T.);
#2781=ORIENTED_EDGE('',*,*,#2213,.T.);
#2782=ORIENTED_EDGE('',*,*,#2209,.T.);
#2783=ORIENTED_EDGE('',*,*,#2203,.T.);
#2784=ORIENTED_EDGE('',*,*,#2208,.T.);
#2785=ORIENTED_EDGE('',*,*,#2214,.T.);
#2786=ORIENTED_EDGE('',*,*,#2193,.T.);
#2787=ORIENTED_EDGE('',*,*,#2186,.T.);
#2788=ORIENTED_EDGE('',*,*,#2211,.F.);
#2789=ORIENTED_EDGE('',*,*,#2165,.T.);
#2790=ORIENTED_EDGE('',*,*,#2215,.F.);
#2791=ORIENTED_EDGE('',*,*,#2216,.T.);
#2792=ORIENTED_EDGE('',*,*,#2182,.T.);
#2793=ORIENTED_EDGE('',*,*,#2216,.F.);
#2794=ORIENTED_EDGE('',*,*,#2217,.T.);
#2795=ORIENTED_EDGE('',*,*,#2191,.T.);
#2796=ORIENTED_EDGE('',*,*,#2194,.T.);
#2797=ORIENTED_EDGE('',*,*,#2214,.F.);
#2798=ORIENTED_EDGE('',*,*,#2207,.T.);
#2799=ORIENTED_EDGE('',*,*,#2210,.T.);
#2800=ORIENTED_EDGE('',*,*,#2213,.F.);
#2801=ORIENTED_EDGE('',*,*,#2199,.T.);
#2802=ORIENTED_EDGE('',*,*,#2202,.T.);
#2803=ORIENTED_EDGE('',*,*,#2212,.F.);
#2804=ORIENTED_EDGE('',*,*,#2217,.F.);
#2805=ORIENTED_EDGE('',*,*,#2218,.T.);
#2806=ORIENTED_EDGE('',*,*,#2219,.T.);
#2807=ORIENTED_EDGE('',*,*,#2218,.F.);
#2808=ORIENTED_EDGE('',*,*,#2220,.F.);
#2809=ORIENTED_EDGE('',*,*,#2221,.T.);
#2810=ORIENTED_EDGE('',*,*,#2222,.T.);
#2811=ORIENTED_EDGE('',*,*,#2221,.F.);
#2812=ORIENTED_EDGE('',*,*,#2215,.T.);
#2813=ORIENTED_EDGE('',*,*,#2162,.T.);
#2814=ORIENTED_EDGE('',*,*,#2171,.T.);
#2815=ORIENTED_EDGE('',*,*,#2179,.T.);
#2816=ORIENTED_EDGE('',*,*,#2220,.T.);
#2817=ORIENTED_EDGE('',*,*,#2219,.F.);
#2818=ORIENTED_EDGE('',*,*,#2189,.T.);
#2819=ORIENTED_EDGE('',*,*,#2197,.T.);
#2820=ORIENTED_EDGE('',*,*,#2205,.T.);
#2821=ORIENTED_EDGE('',*,*,#2222,.F.);
#2822=ORIENTED_EDGE('',*,*,#2223,.F.);
#2823=ORIENTED_EDGE('',*,*,#2224,.T.);
#2824=ORIENTED_EDGE('',*,*,#2225,.F.);
#2825=ORIENTED_EDGE('',*,*,#2224,.F.);
#2826=ORIENTED_EDGE('',*,*,#2223,.T.);
#2827=ORIENTED_EDGE('',*,*,#2226,.F.);
#2828=ORIENTED_EDGE('',*,*,#2227,.T.);
#2829=ORIENTED_EDGE('',*,*,#2228,.F.);
#2830=ORIENTED_EDGE('',*,*,#2227,.F.);
#2831=ORIENTED_EDGE('',*,*,#2226,.T.);
#2832=ORIENTED_EDGE('',*,*,#2229,.F.);
#2833=ORIENTED_EDGE('',*,*,#2230,.T.);
#2834=ORIENTED_EDGE('',*,*,#2231,.T.);
#2835=ORIENTED_EDGE('',*,*,#2230,.F.);
#2836=ORIENTED_EDGE('',*,*,#2231,.F.);
#2837=ORIENTED_EDGE('',*,*,#2232,.F.);
#2838=ORIENTED_EDGE('',*,*,#2233,.T.);
#2839=ORIENTED_EDGE('',*,*,#2234,.T.);
#2840=ORIENTED_EDGE('',*,*,#2233,.F.);
#2841=ORIENTED_EDGE('',*,*,#2234,.F.);
#2842=ORIENTED_EDGE('',*,*,#2235,.F.);
#2843=ORIENTED_EDGE('',*,*,#2236,.F.);
#2844=ORIENTED_EDGE('',*,*,#2237,.F.);
#2845=ORIENTED_EDGE('',*,*,#2238,.F.);
#2846=ORIENTED_EDGE('',*,*,#2237,.T.);
#2847=ORIENTED_EDGE('',*,*,#2239,.F.);
#2848=ORIENTED_EDGE('',*,*,#2240,.F.);
#2849=ORIENTED_EDGE('',*,*,#2241,.T.);
#2850=ORIENTED_EDGE('',*,*,#2242,.T.);
#2851=ORIENTED_EDGE('',*,*,#2243,.F.);
#2852=ORIENTED_EDGE('',*,*,#2236,.T.);
#2853=ORIENTED_EDGE('',*,*,#2244,.T.);
#2854=ORIENTED_EDGE('',*,*,#2245,.T.);
#2855=ORIENTED_EDGE('',*,*,#2239,.T.);
#2856=ORIENTED_EDGE('',*,*,#2225,.T.);
#2857=ORIENTED_EDGE('',*,*,#2246,.T.);
#2858=ORIENTED_EDGE('',*,*,#2247,.T.);
#2859=ORIENTED_EDGE('',*,*,#2248,.F.);
#2860=ORIENTED_EDGE('',*,*,#2242,.F.);
#2861=ORIENTED_EDGE('',*,*,#2249,.T.);
#2862=ORIENTED_EDGE('',*,*,#2240,.T.);
#2863=ORIENTED_EDGE('',*,*,#2245,.F.);
#2864=ORIENTED_EDGE('',*,*,#2250,.F.);
#2865=ORIENTED_EDGE('',*,*,#2235,.T.);
#2866=ORIENTED_EDGE('',*,*,#2251,.F.);
#2867=ORIENTED_EDGE('',*,*,#2247,.F.);
#2868=ORIENTED_EDGE('',*,*,#2252,.T.);
#2869=ORIENTED_EDGE('',*,*,#2250,.T.);
#2870=ORIENTED_EDGE('',*,*,#2244,.F.);
#2871=ORIENTED_EDGE('',*,*,#2238,.T.);
#2872=ORIENTED_EDGE('',*,*,#2243,.T.);
#2873=ORIENTED_EDGE('',*,*,#2248,.T.);
#2874=ORIENTED_EDGE('',*,*,#2251,.T.);
#2875=ORIENTED_EDGE('',*,*,#2228,.T.);
#2876=ORIENTED_EDGE('',*,*,#2252,.F.);
#2877=ORIENTED_EDGE('',*,*,#2246,.F.);
#2878=ORIENTED_EDGE('',*,*,#2241,.F.);
#2879=ORIENTED_EDGE('',*,*,#2249,.F.);
#2880=ORIENTED_EDGE('',*,*,#2229,.T.);
#2881=ORIENTED_EDGE('',*,*,#2232,.T.);
#2882=ORIENTED_EDGE('',*,*,#2253,.F.);
#2883=ORIENTED_EDGE('',*,*,#2254,.T.);
#2884=ORIENTED_EDGE('',*,*,#2255,.F.);
#2885=ORIENTED_EDGE('',*,*,#2256,.F.);
#2886=ORIENTED_EDGE('',*,*,#2257,.F.);
#2887=ORIENTED_EDGE('',*,*,#2258,.F.);
#2888=ORIENTED_EDGE('',*,*,#2254,.F.);
#2889=ORIENTED_EDGE('',*,*,#2259,.F.);
#2890=ORIENTED_EDGE('',*,*,#2260,.T.);
#2891=ORIENTED_EDGE('',*,*,#2261,.F.);
#2892=ORIENTED_EDGE('',*,*,#2262,.F.);
#2893=ORIENTED_EDGE('',*,*,#2263,.F.);
#2894=ORIENTED_EDGE('',*,*,#2264,.F.);
#2895=ORIENTED_EDGE('',*,*,#2260,.F.);
#2896=ORIENTED_EDGE('',*,*,#2256,.T.);
#2897=ORIENTED_EDGE('',*,*,#2253,.T.);
#2898=ORIENTED_EDGE('',*,*,#2258,.T.);
#2899=ORIENTED_EDGE('',*,*,#2265,.F.);
#2900=ORIENTED_EDGE('',*,*,#2266,.F.);
#2901=ORIENTED_EDGE('',*,*,#2267,.T.);
#2902=ORIENTED_EDGE('',*,*,#2268,.T.);
#2903=ORIENTED_EDGE('',*,*,#2269,.F.);
#2904=ORIENTED_EDGE('',*,*,#2262,.T.);
#2905=ORIENTED_EDGE('',*,*,#2259,.T.);
#2906=ORIENTED_EDGE('',*,*,#2264,.T.);
#2907=ORIENTED_EDGE('',*,*,#2270,.F.);
#2908=ORIENTED_EDGE('',*,*,#2271,.F.);
#2909=ORIENTED_EDGE('',*,*,#2272,.T.);
#2910=ORIENTED_EDGE('',*,*,#2273,.T.);
#2911=ORIENTED_EDGE('',*,*,#2274,.F.);
#2912=ORIENTED_EDGE('',*,*,#2275,.F.);
#2913=ORIENTED_EDGE('',*,*,#2276,.T.);
#2914=ORIENTED_EDGE('',*,*,#2255,.T.);
#2915=ORIENTED_EDGE('',*,*,#2276,.F.);
#2916=ORIENTED_EDGE('',*,*,#2277,.F.);
#2917=ORIENTED_EDGE('',*,*,#2278,.T.);
#2918=ORIENTED_EDGE('',*,*,#2261,.T.);
#2919=ORIENTED_EDGE('',*,*,#2278,.F.);
#2920=ORIENTED_EDGE('',*,*,#2279,.F.);
#2921=ORIENTED_EDGE('',*,*,#2280,.F.);
#2922=ORIENTED_EDGE('',*,*,#2281,.F.);
#2923=ORIENTED_EDGE('',*,*,#2282,.F.);
#2924=ORIENTED_EDGE('',*,*,#2281,.T.);
#2925=ORIENTED_EDGE('',*,*,#2283,.T.);
#2926=ORIENTED_EDGE('',*,*,#2271,.T.);
#2927=ORIENTED_EDGE('',*,*,#2284,.F.);
#2928=ORIENTED_EDGE('',*,*,#2268,.F.);
#2929=ORIENTED_EDGE('',*,*,#2285,.T.);
#2930=ORIENTED_EDGE('',*,*,#2280,.T.);
#2931=ORIENTED_EDGE('',*,*,#2286,.F.);
#2932=ORIENTED_EDGE('',*,*,#2272,.F.);
#2933=ORIENTED_EDGE('',*,*,#2283,.F.);
#2934=ORIENTED_EDGE('',*,*,#2277,.T.);
#2935=ORIENTED_EDGE('',*,*,#2279,.T.);
#2936=ORIENTED_EDGE('',*,*,#2287,.T.);
#2937=ORIENTED_EDGE('',*,*,#2266,.T.);
#2938=ORIENTED_EDGE('',*,*,#2288,.F.);
#2939=ORIENTED_EDGE('',*,*,#2273,.F.);
#2940=ORIENTED_EDGE('',*,*,#2286,.T.);
#2941=ORIENTED_EDGE('',*,*,#2257,.T.);
#2942=ORIENTED_EDGE('',*,*,#2269,.T.);
#2943=ORIENTED_EDGE('',*,*,#2284,.T.);
#2944=ORIENTED_EDGE('',*,*,#2270,.T.);
#2945=ORIENTED_EDGE('',*,*,#2263,.T.);
#2946=ORIENTED_EDGE('',*,*,#2274,.T.);
#2947=ORIENTED_EDGE('',*,*,#2288,.T.);
#2948=ORIENTED_EDGE('',*,*,#2265,.T.);
#2949=ORIENTED_EDGE('',*,*,#2282,.T.);
#2950=ORIENTED_EDGE('',*,*,#2285,.F.);
#2951=ORIENTED_EDGE('',*,*,#2267,.F.);
#2952=ORIENTED_EDGE('',*,*,#2287,.F.);
#2953=ORIENTED_EDGE('',*,*,#2275,.T.);
#2954=ORIENTED_EDGE('',*,*,#2289,.F.);
#2955=ORIENTED_EDGE('',*,*,#2290,.T.);
#2956=ORIENTED_EDGE('',*,*,#2291,.F.);
#2957=ORIENTED_EDGE('',*,*,#2290,.F.);
#2958=ORIENTED_EDGE('',*,*,#2289,.T.);
#2959=ORIENTED_EDGE('',*,*,#2292,.F.);
#2960=ORIENTED_EDGE('',*,*,#2293,.T.);
#2961=ORIENTED_EDGE('',*,*,#2294,.F.);
#2962=ORIENTED_EDGE('',*,*,#2293,.F.);
#2963=ORIENTED_EDGE('',*,*,#2292,.T.);
#2964=ORIENTED_EDGE('',*,*,#2295,.F.);
#2965=ORIENTED_EDGE('',*,*,#2296,.T.);
#2966=ORIENTED_EDGE('',*,*,#2297,.T.);
#2967=ORIENTED_EDGE('',*,*,#2296,.F.);
#2968=ORIENTED_EDGE('',*,*,#2297,.F.);
#2969=ORIENTED_EDGE('',*,*,#2298,.F.);
#2970=ORIENTED_EDGE('',*,*,#2299,.T.);
#2971=ORIENTED_EDGE('',*,*,#2300,.T.);
#2972=ORIENTED_EDGE('',*,*,#2299,.F.);
#2973=ORIENTED_EDGE('',*,*,#2300,.F.);
#2974=ORIENTED_EDGE('',*,*,#2301,.F.);
#2975=ORIENTED_EDGE('',*,*,#2302,.F.);
#2976=ORIENTED_EDGE('',*,*,#2303,.F.);
#2977=ORIENTED_EDGE('',*,*,#2304,.F.);
#2978=ORIENTED_EDGE('',*,*,#2303,.T.);
#2979=ORIENTED_EDGE('',*,*,#2305,.F.);
#2980=ORIENTED_EDGE('',*,*,#2306,.F.);
#2981=ORIENTED_EDGE('',*,*,#2307,.T.);
#2982=ORIENTED_EDGE('',*,*,#2308,.T.);
#2983=ORIENTED_EDGE('',*,*,#2309,.F.);
#2984=ORIENTED_EDGE('',*,*,#2302,.T.);
#2985=ORIENTED_EDGE('',*,*,#2310,.T.);
#2986=ORIENTED_EDGE('',*,*,#2311,.T.);
#2987=ORIENTED_EDGE('',*,*,#2305,.T.);
#2988=ORIENTED_EDGE('',*,*,#2291,.T.);
#2989=ORIENTED_EDGE('',*,*,#2312,.T.);
#2990=ORIENTED_EDGE('',*,*,#2313,.T.);
#2991=ORIENTED_EDGE('',*,*,#2314,.F.);
#2992=ORIENTED_EDGE('',*,*,#2308,.F.);
#2993=ORIENTED_EDGE('',*,*,#2315,.T.);
#2994=ORIENTED_EDGE('',*,*,#2306,.T.);
#2995=ORIENTED_EDGE('',*,*,#2311,.F.);
#2996=ORIENTED_EDGE('',*,*,#2316,.F.);
#2997=ORIENTED_EDGE('',*,*,#2301,.T.);
#2998=ORIENTED_EDGE('',*,*,#2317,.F.);
#2999=ORIENTED_EDGE('',*,*,#2313,.F.);
#3000=ORIENTED_EDGE('',*,*,#2318,.T.);
#3001=ORIENTED_EDGE('',*,*,#2316,.T.);
#3002=ORIENTED_EDGE('',*,*,#2310,.F.);
#3003=ORIENTED_EDGE('',*,*,#2304,.T.);
#3004=ORIENTED_EDGE('',*,*,#2309,.T.);
#3005=ORIENTED_EDGE('',*,*,#2314,.T.);
#3006=ORIENTED_EDGE('',*,*,#2317,.T.);
#3007=ORIENTED_EDGE('',*,*,#2294,.T.);
#3008=ORIENTED_EDGE('',*,*,#2318,.F.);
#3009=ORIENTED_EDGE('',*,*,#2312,.F.);
#3010=ORIENTED_EDGE('',*,*,#2307,.F.);
#3011=ORIENTED_EDGE('',*,*,#2315,.F.);
#3012=ORIENTED_EDGE('',*,*,#2295,.T.);
#3013=ORIENTED_EDGE('',*,*,#2298,.T.);
#3014=ORIENTED_EDGE('',*,*,#2319,.F.);
#3015=ORIENTED_EDGE('',*,*,#2320,.T.);
#3016=ORIENTED_EDGE('',*,*,#2321,.F.);
#3017=ORIENTED_EDGE('',*,*,#2322,.F.);
#3018=ORIENTED_EDGE('',*,*,#2323,.F.);
#3019=ORIENTED_EDGE('',*,*,#2324,.F.);
#3020=ORIENTED_EDGE('',*,*,#2320,.F.);
#3021=ORIENTED_EDGE('',*,*,#2325,.F.);
#3022=ORIENTED_EDGE('',*,*,#2326,.T.);
#3023=ORIENTED_EDGE('',*,*,#2327,.F.);
#3024=ORIENTED_EDGE('',*,*,#2328,.F.);
#3025=ORIENTED_EDGE('',*,*,#2329,.F.);
#3026=ORIENTED_EDGE('',*,*,#2330,.F.);
#3027=ORIENTED_EDGE('',*,*,#2326,.F.);
#3028=ORIENTED_EDGE('',*,*,#2322,.T.);
#3029=ORIENTED_EDGE('',*,*,#2319,.T.);
#3030=ORIENTED_EDGE('',*,*,#2324,.T.);
#3031=ORIENTED_EDGE('',*,*,#2331,.F.);
#3032=ORIENTED_EDGE('',*,*,#2332,.F.);
#3033=ORIENTED_EDGE('',*,*,#2333,.T.);
#3034=ORIENTED_EDGE('',*,*,#2334,.T.);
#3035=ORIENTED_EDGE('',*,*,#2335,.F.);
#3036=ORIENTED_EDGE('',*,*,#2328,.T.);
#3037=ORIENTED_EDGE('',*,*,#2325,.T.);
#3038=ORIENTED_EDGE('',*,*,#2330,.T.);
#3039=ORIENTED_EDGE('',*,*,#2336,.F.);
#3040=ORIENTED_EDGE('',*,*,#2337,.F.);
#3041=ORIENTED_EDGE('',*,*,#2338,.T.);
#3042=ORIENTED_EDGE('',*,*,#2339,.T.);
#3043=ORIENTED_EDGE('',*,*,#2340,.F.);
#3044=ORIENTED_EDGE('',*,*,#2341,.F.);
#3045=ORIENTED_EDGE('',*,*,#2342,.T.);
#3046=ORIENTED_EDGE('',*,*,#2321,.T.);
#3047=ORIENTED_EDGE('',*,*,#2342,.F.);
#3048=ORIENTED_EDGE('',*,*,#2343,.F.);
#3049=ORIENTED_EDGE('',*,*,#2344,.T.);
#3050=ORIENTED_EDGE('',*,*,#2327,.T.);
#3051=ORIENTED_EDGE('',*,*,#2344,.F.);
#3052=ORIENTED_EDGE('',*,*,#2345,.F.);
#3053=ORIENTED_EDGE('',*,*,#2346,.F.);
#3054=ORIENTED_EDGE('',*,*,#2347,.F.);
#3055=ORIENTED_EDGE('',*,*,#2348,.F.);
#3056=ORIENTED_EDGE('',*,*,#2347,.T.);
#3057=ORIENTED_EDGE('',*,*,#2349,.T.);
#3058=ORIENTED_EDGE('',*,*,#2337,.T.);
#3059=ORIENTED_EDGE('',*,*,#2350,.F.);
#3060=ORIENTED_EDGE('',*,*,#2334,.F.);
#3061=ORIENTED_EDGE('',*,*,#2351,.T.);
#3062=ORIENTED_EDGE('',*,*,#2346,.T.);
#3063=ORIENTED_EDGE('',*,*,#2352,.F.);
#3064=ORIENTED_EDGE('',*,*,#2338,.F.);
#3065=ORIENTED_EDGE('',*,*,#2349,.F.);
#3066=ORIENTED_EDGE('',*,*,#2343,.T.);
#3067=ORIENTED_EDGE('',*,*,#2345,.T.);
#3068=ORIENTED_EDGE('',*,*,#2353,.T.);
#3069=ORIENTED_EDGE('',*,*,#2332,.T.);
#3070=ORIENTED_EDGE('',*,*,#2354,.F.);
#3071=ORIENTED_EDGE('',*,*,#2339,.F.);
#3072=ORIENTED_EDGE('',*,*,#2352,.T.);
#3073=ORIENTED_EDGE('',*,*,#2323,.T.);
#3074=ORIENTED_EDGE('',*,*,#2335,.T.);
#3075=ORIENTED_EDGE('',*,*,#2350,.T.);
#3076=ORIENTED_EDGE('',*,*,#2336,.T.);
#3077=ORIENTED_EDGE('',*,*,#2329,.T.);
#3078=ORIENTED_EDGE('',*,*,#2340,.T.);
#3079=ORIENTED_EDGE('',*,*,#2354,.T.);
#3080=ORIENTED_EDGE('',*,*,#2331,.T.);
#3081=ORIENTED_EDGE('',*,*,#2348,.T.);
#3082=ORIENTED_EDGE('',*,*,#2351,.F.);
#3083=ORIENTED_EDGE('',*,*,#2333,.F.);
#3084=ORIENTED_EDGE('',*,*,#2353,.F.);
#3085=ORIENTED_EDGE('',*,*,#2341,.T.);
#3086=ORIENTED_EDGE('',*,*,#2355,.F.);
#3087=ORIENTED_EDGE('',*,*,#2356,.T.);
#3088=ORIENTED_EDGE('',*,*,#2357,.T.);
#3089=ORIENTED_EDGE('',*,*,#2356,.F.);
#3090=ORIENTED_EDGE('',*,*,#2358,.F.);
#3091=ORIENTED_EDGE('',*,*,#2359,.T.);
#3092=ORIENTED_EDGE('',*,*,#2360,.T.);
#3093=ORIENTED_EDGE('',*,*,#2359,.F.);
#3094=ORIENTED_EDGE('',*,*,#2358,.T.);
#3095=ORIENTED_EDGE('',*,*,#2355,.T.);
#3096=ORIENTED_EDGE('',*,*,#2360,.F.);
#3097=ORIENTED_EDGE('',*,*,#2357,.F.);
#3098=ORIENTED_EDGE('',*,*,#2361,.F.);
#3099=ORIENTED_EDGE('',*,*,#2362,.T.);
#3100=ORIENTED_EDGE('',*,*,#2363,.T.);
#3101=ORIENTED_EDGE('',*,*,#2362,.F.);
#3102=ORIENTED_EDGE('',*,*,#2364,.F.);
#3103=ORIENTED_EDGE('',*,*,#2365,.T.);
#3104=ORIENTED_EDGE('',*,*,#2366,.T.);
#3105=ORIENTED_EDGE('',*,*,#2365,.F.);
#3106=ORIENTED_EDGE('',*,*,#2364,.T.);
#3107=ORIENTED_EDGE('',*,*,#2361,.T.);
#3108=ORIENTED_EDGE('',*,*,#2366,.F.);
#3109=ORIENTED_EDGE('',*,*,#2363,.F.);
#3110=ORIENTED_EDGE('',*,*,#2367,.F.);
#3111=ORIENTED_EDGE('',*,*,#2368,.T.);
#3112=ORIENTED_EDGE('',*,*,#2369,.T.);
#3113=ORIENTED_EDGE('',*,*,#2368,.F.);
#3114=ORIENTED_EDGE('',*,*,#2370,.F.);
#3115=ORIENTED_EDGE('',*,*,#2371,.T.);
#3116=ORIENTED_EDGE('',*,*,#2372,.T.);
#3117=ORIENTED_EDGE('',*,*,#2371,.F.);
#3118=ORIENTED_EDGE('',*,*,#2370,.T.);
#3119=ORIENTED_EDGE('',*,*,#2367,.T.);
#3120=ORIENTED_EDGE('',*,*,#2372,.F.);
#3121=ORIENTED_EDGE('',*,*,#2369,.F.);
#3122=ORIENTED_EDGE('',*,*,#2373,.F.);
#3123=ORIENTED_EDGE('',*,*,#2374,.T.);
#3124=ORIENTED_EDGE('',*,*,#2375,.F.);
#3125=ORIENTED_EDGE('',*,*,#2374,.F.);
#3126=ORIENTED_EDGE('',*,*,#2376,.F.);
#3127=ORIENTED_EDGE('',*,*,#2377,.T.);
#3128=ORIENTED_EDGE('',*,*,#2378,.F.);
#3129=ORIENTED_EDGE('',*,*,#2377,.F.);
#3130=ORIENTED_EDGE('',*,*,#2379,.F.);
#3131=ORIENTED_EDGE('',*,*,#2380,.T.);
#3132=ORIENTED_EDGE('',*,*,#2381,.F.);
#3133=ORIENTED_EDGE('',*,*,#2380,.F.);
#3134=ORIENTED_EDGE('',*,*,#2382,.F.);
#3135=ORIENTED_EDGE('',*,*,#2383,.T.);
#3136=ORIENTED_EDGE('',*,*,#2384,.T.);
#3137=ORIENTED_EDGE('',*,*,#2383,.F.);
#3138=ORIENTED_EDGE('',*,*,#2384,.F.);
#3139=ORIENTED_EDGE('',*,*,#2385,.F.);
#3140=ORIENTED_EDGE('',*,*,#2386,.F.);
#3141=ORIENTED_EDGE('',*,*,#2387,.T.);
#3142=ORIENTED_EDGE('',*,*,#2385,.T.);
#3143=ORIENTED_EDGE('',*,*,#2387,.F.);
#3144=ORIENTED_EDGE('',*,*,#2388,.F.);
#3145=ORIENTED_EDGE('',*,*,#2389,.T.);
#3146=ORIENTED_EDGE('',*,*,#2390,.T.);
#3147=ORIENTED_EDGE('',*,*,#2389,.F.);
#3148=ORIENTED_EDGE('',*,*,#2388,.T.);
#3149=ORIENTED_EDGE('',*,*,#2375,.T.);
#3150=ORIENTED_EDGE('',*,*,#2378,.T.);
#3151=ORIENTED_EDGE('',*,*,#2381,.T.);
#3152=ORIENTED_EDGE('',*,*,#2386,.T.);
#3153=ORIENTED_EDGE('',*,*,#2390,.F.);
#3154=ORIENTED_EDGE('',*,*,#2373,.T.);
#3155=ORIENTED_EDGE('',*,*,#2376,.T.);
#3156=ORIENTED_EDGE('',*,*,#2379,.T.);
#3157=ORIENTED_EDGE('',*,*,#2382,.T.);
#3158=ORIENTED_EDGE('',*,*,#2391,.F.);
#3159=ORIENTED_EDGE('',*,*,#2392,.F.);
#3160=ORIENTED_EDGE('',*,*,#2393,.F.);
#3161=ORIENTED_EDGE('',*,*,#2394,.T.);
#3162=ORIENTED_EDGE('',*,*,#2395,.F.);
#3163=ORIENTED_EDGE('',*,*,#2392,.T.);
#3164=ORIENTED_EDGE('',*,*,#2396,.F.);
#3165=ORIENTED_EDGE('',*,*,#2394,.F.);
#3166=ORIENTED_EDGE('',*,*,#2397,.F.);
#3167=ORIENTED_EDGE('',*,*,#2398,.F.);
#3168=ORIENTED_EDGE('',*,*,#2399,.T.);
#3169=ORIENTED_EDGE('',*,*,#2400,.F.);
#3170=ORIENTED_EDGE('',*,*,#2399,.F.);
#3171=ORIENTED_EDGE('',*,*,#2401,.F.);
#3172=ORIENTED_EDGE('',*,*,#2402,.F.);
#3173=ORIENTED_EDGE('',*,*,#2403,.F.);
#3174=ORIENTED_EDGE('',*,*,#2404,.T.);
#3175=ORIENTED_EDGE('',*,*,#2405,.F.);
#3176=ORIENTED_EDGE('',*,*,#2406,.F.);
#3177=ORIENTED_EDGE('',*,*,#2402,.T.);
#3178=ORIENTED_EDGE('',*,*,#2407,.F.);
#3179=ORIENTED_EDGE('',*,*,#2408,.F.);
#3180=ORIENTED_EDGE('',*,*,#2404,.F.);
#3181=ORIENTED_EDGE('',*,*,#2409,.F.);
#3182=ORIENTED_EDGE('',*,*,#2410,.F.);
#3183=ORIENTED_EDGE('',*,*,#2411,.F.);
#3184=ORIENTED_EDGE('',*,*,#2412,.T.);
#3185=ORIENTED_EDGE('',*,*,#2413,.F.);
#3186=ORIENTED_EDGE('',*,*,#2414,.F.);
#3187=ORIENTED_EDGE('',*,*,#2410,.T.);
#3188=ORIENTED_EDGE('',*,*,#2415,.F.);
#3189=ORIENTED_EDGE('',*,*,#2416,.F.);
#3190=ORIENTED_EDGE('',*,*,#2412,.F.);
#3191=ORIENTED_EDGE('',*,*,#2417,.F.);
#3192=ORIENTED_EDGE('',*,*,#2418,.F.);
#3193=ORIENTED_EDGE('',*,*,#2419,.F.);
#3194=ORIENTED_EDGE('',*,*,#2420,.T.);
#3195=ORIENTED_EDGE('',*,*,#2421,.F.);
#3196=ORIENTED_EDGE('',*,*,#2422,.F.);
#3197=ORIENTED_EDGE('',*,*,#2418,.T.);
#3198=ORIENTED_EDGE('',*,*,#2423,.F.);
#3199=ORIENTED_EDGE('',*,*,#2424,.F.);
#3200=ORIENTED_EDGE('',*,*,#2420,.F.);
#3201=ORIENTED_EDGE('',*,*,#2407,.T.);
#3202=ORIENTED_EDGE('',*,*,#2401,.T.);
#3203=ORIENTED_EDGE('',*,*,#2406,.T.);
#3204=ORIENTED_EDGE('',*,*,#2425,.F.);
#3205=ORIENTED_EDGE('',*,*,#2415,.T.);
#3206=ORIENTED_EDGE('',*,*,#2409,.T.);
#3207=ORIENTED_EDGE('',*,*,#2414,.T.);
#3208=ORIENTED_EDGE('',*,*,#2426,.F.);
#3209=ORIENTED_EDGE('',*,*,#2423,.T.);
#3210=ORIENTED_EDGE('',*,*,#2417,.T.);
#3211=ORIENTED_EDGE('',*,*,#2422,.T.);
#3212=ORIENTED_EDGE('',*,*,#2427,.F.);
#3213=ORIENTED_EDGE('',*,*,#2428,.T.);
#3214=ORIENTED_EDGE('',*,*,#2429,.F.);
#3215=ORIENTED_EDGE('',*,*,#2430,.T.);
#3216=ORIENTED_EDGE('',*,*,#2431,.F.);
#3217=ORIENTED_EDGE('',*,*,#2395,.T.);
#3218=ORIENTED_EDGE('',*,*,#2396,.T.);
#3219=ORIENTED_EDGE('',*,*,#2391,.T.);
#3220=ORIENTED_EDGE('',*,*,#2397,.T.);
#3221=ORIENTED_EDGE('',*,*,#2398,.T.);
#3222=ORIENTED_EDGE('',*,*,#2432,.F.);
#3223=ORIENTED_EDGE('',*,*,#2433,.F.);
#3224=ORIENTED_EDGE('',*,*,#2430,.F.);
#3225=ORIENTED_EDGE('',*,*,#2434,.F.);
#3226=ORIENTED_EDGE('',*,*,#2393,.T.);
#3227=ORIENTED_EDGE('',*,*,#2435,.F.);
#3228=ORIENTED_EDGE('',*,*,#2436,.F.);
#3229=ORIENTED_EDGE('',*,*,#2428,.F.);
#3230=ORIENTED_EDGE('',*,*,#2437,.F.);
#3231=ORIENTED_EDGE('',*,*,#2400,.T.);
#3232=ORIENTED_EDGE('',*,*,#2438,.T.);
#3233=ORIENTED_EDGE('',*,*,#2405,.T.);
#3234=ORIENTED_EDGE('',*,*,#2408,.T.);
#3235=ORIENTED_EDGE('',*,*,#2431,.T.);
#3236=ORIENTED_EDGE('',*,*,#2433,.T.);
#3237=ORIENTED_EDGE('',*,*,#2439,.F.);
#3238=ORIENTED_EDGE('',*,*,#2437,.T.);
#3239=ORIENTED_EDGE('',*,*,#2427,.T.);
#3240=ORIENTED_EDGE('',*,*,#2421,.T.);
#3241=ORIENTED_EDGE('',*,*,#2424,.T.);
#3242=ORIENTED_EDGE('',*,*,#2426,.T.);
#3243=ORIENTED_EDGE('',*,*,#2413,.T.);
#3244=ORIENTED_EDGE('',*,*,#2416,.T.);
#3245=ORIENTED_EDGE('',*,*,#2425,.T.);
#3246=ORIENTED_EDGE('',*,*,#2434,.T.);
#3247=ORIENTED_EDGE('',*,*,#2429,.T.);
#3248=ORIENTED_EDGE('',*,*,#2436,.T.);
#3249=ORIENTED_EDGE('',*,*,#2440,.T.);
#3250=ORIENTED_EDGE('',*,*,#2441,.T.);
#3251=ORIENTED_EDGE('',*,*,#2432,.T.);
#3252=ORIENTED_EDGE('',*,*,#2441,.F.);
#3253=ORIENTED_EDGE('',*,*,#2442,.T.);
#3254=ORIENTED_EDGE('',*,*,#2443,.T.);
#3255=ORIENTED_EDGE('',*,*,#2442,.F.);
#3256=ORIENTED_EDGE('',*,*,#2440,.F.);
#3257=ORIENTED_EDGE('',*,*,#2435,.T.);
#3258=ORIENTED_EDGE('',*,*,#2439,.T.);
#3259=ORIENTED_EDGE('',*,*,#2438,.F.);
#3260=ORIENTED_EDGE('',*,*,#2444,.T.);
#3261=ORIENTED_EDGE('',*,*,#2445,.T.);
#3262=ORIENTED_EDGE('',*,*,#2444,.F.);
#3263=ORIENTED_EDGE('',*,*,#2445,.F.);
#3264=ORIENTED_EDGE('',*,*,#2403,.T.);
#3265=ORIENTED_EDGE('',*,*,#2411,.T.);
#3266=ORIENTED_EDGE('',*,*,#2419,.T.);
#3267=ORIENTED_EDGE('',*,*,#2443,.F.);
#3268=ORIENTED_EDGE('',*,*,#2446,.F.);
#3269=ORIENTED_EDGE('',*,*,#2447,.F.);
#3270=ORIENTED_EDGE('',*,*,#2448,.T.);
#3271=ORIENTED_EDGE('',*,*,#2446,.T.);
#3272=ORIENTED_EDGE('',*,*,#2448,.F.);
#3273=ORIENTED_EDGE('',*,*,#2449,.F.);
#3274=ORIENTED_EDGE('',*,*,#2450,.T.);
#3275=ORIENTED_EDGE('',*,*,#2447,.T.);
#3276=ORIENTED_EDGE('',*,*,#2450,.F.);
#3277=ORIENTED_EDGE('',*,*,#2451,.F.);
#3278=ORIENTED_EDGE('',*,*,#2452,.T.);
#3279=ORIENTED_EDGE('',*,*,#2449,.T.);
#3280=ORIENTED_EDGE('',*,*,#2452,.F.);
#3281=ORIENTED_EDGE('',*,*,#2451,.T.);
#3282=ORIENTED_EDGE('',*,*,#2453,.F.);
#3283=ORIENTED_EDGE('',*,*,#2454,.F.);
#3284=ORIENTED_EDGE('',*,*,#2455,.T.);
#3285=ORIENTED_EDGE('',*,*,#2453,.T.);
#3286=ORIENTED_EDGE('',*,*,#2455,.F.);
#3287=ORIENTED_EDGE('',*,*,#2456,.F.);
#3288=ORIENTED_EDGE('',*,*,#2457,.T.);
#3289=ORIENTED_EDGE('',*,*,#2454,.T.);
#3290=ORIENTED_EDGE('',*,*,#2457,.F.);
#3291=ORIENTED_EDGE('',*,*,#2458,.F.);
#3292=ORIENTED_EDGE('',*,*,#2459,.T.);
#3293=ORIENTED_EDGE('',*,*,#2456,.T.);
#3294=ORIENTED_EDGE('',*,*,#2459,.F.);
#3295=ORIENTED_EDGE('',*,*,#2458,.T.);
#3296=ORIENTED_EDGE('',*,*,#2460,.T.);
#3297=ORIENTED_EDGE('',*,*,#2461,.T.);
#3298=ORIENTED_EDGE('',*,*,#2462,.T.);
#3299=ORIENTED_EDGE('',*,*,#2463,.F.);
#3300=ORIENTED_EDGE('',*,*,#2464,.T.);
#3301=ORIENTED_EDGE('',*,*,#2465,.T.);
#3302=ORIENTED_EDGE('',*,*,#2466,.T.);
#3303=ORIENTED_EDGE('',*,*,#2461,.F.);
#3304=ORIENTED_EDGE('',*,*,#2467,.T.);
#3305=ORIENTED_EDGE('',*,*,#2468,.T.);
#3306=ORIENTED_EDGE('',*,*,#2469,.T.);
#3307=ORIENTED_EDGE('',*,*,#2465,.F.);
#3308=ORIENTED_EDGE('',*,*,#2470,.T.);
#3309=ORIENTED_EDGE('',*,*,#2471,.T.);
#3310=ORIENTED_EDGE('',*,*,#2472,.T.);
#3311=ORIENTED_EDGE('',*,*,#2468,.F.);
#3312=ORIENTED_EDGE('',*,*,#2473,.T.);
#3313=ORIENTED_EDGE('',*,*,#2474,.T.);
#3314=ORIENTED_EDGE('',*,*,#2475,.T.);
#3315=ORIENTED_EDGE('',*,*,#2471,.F.);
#3316=ORIENTED_EDGE('',*,*,#2476,.T.);
#3317=ORIENTED_EDGE('',*,*,#2463,.T.);
#3318=ORIENTED_EDGE('',*,*,#2477,.T.);
#3319=ORIENTED_EDGE('',*,*,#2474,.F.);
#3320=ORIENTED_EDGE('',*,*,#2476,.F.);
#3321=ORIENTED_EDGE('',*,*,#2473,.F.);
#3322=ORIENTED_EDGE('',*,*,#2470,.F.);
#3323=ORIENTED_EDGE('',*,*,#2467,.F.);
#3324=ORIENTED_EDGE('',*,*,#2464,.F.);
#3325=ORIENTED_EDGE('',*,*,#2460,.F.);
#3326=ORIENTED_EDGE('',*,*,#2477,.F.);
#3327=ORIENTED_EDGE('',*,*,#2462,.F.);
#3328=ORIENTED_EDGE('',*,*,#2466,.F.);
#3329=ORIENTED_EDGE('',*,*,#2469,.F.);
#3330=ORIENTED_EDGE('',*,*,#2472,.F.);
#3331=ORIENTED_EDGE('',*,*,#2475,.F.);
#3332=ORIENTED_EDGE('',*,*,#2478,.F.);
#3333=ORIENTED_EDGE('',*,*,#2479,.F.);
#3334=ORIENTED_EDGE('',*,*,#2480,.F.);
#3335=ORIENTED_EDGE('',*,*,#2481,.F.);
#3336=ORIENTED_EDGE('',*,*,#2482,.F.);
#3337=ORIENTED_EDGE('',*,*,#2481,.T.);
#3338=ORIENTED_EDGE('',*,*,#2483,.F.);
#3339=ORIENTED_EDGE('',*,*,#2484,.T.);
#3340=ORIENTED_EDGE('',*,*,#2485,.F.);
#3341=ORIENTED_EDGE('',*,*,#2484,.F.);
#3342=ORIENTED_EDGE('',*,*,#2486,.F.);
#3343=ORIENTED_EDGE('',*,*,#2487,.F.);
#3344=ORIENTED_EDGE('',*,*,#2488,.F.);
#3345=ORIENTED_EDGE('',*,*,#2487,.T.);
#3346=ORIENTED_EDGE('',*,*,#2489,.T.);
#3347=ORIENTED_EDGE('',*,*,#2479,.T.);
#3348=ORIENTED_EDGE('',*,*,#2489,.F.);
#3349=ORIENTED_EDGE('',*,*,#2486,.T.);
#3350=ORIENTED_EDGE('',*,*,#2483,.T.);
#3351=ORIENTED_EDGE('',*,*,#2480,.T.);
#3352=ORIENTED_EDGE('',*,*,#2490,.F.);
#3353=ORIENTED_EDGE('',*,*,#2491,.T.);
#3354=ORIENTED_EDGE('',*,*,#2492,.F.);
#3355=ORIENTED_EDGE('',*,*,#2493,.T.);
#3356=ORIENTED_EDGE('',*,*,#2490,.T.);
#3357=ORIENTED_EDGE('',*,*,#2493,.F.);
#3358=ORIENTED_EDGE('',*,*,#2492,.T.);
#3359=ORIENTED_EDGE('',*,*,#2494,.F.);
#3360=ORIENTED_EDGE('',*,*,#2495,.F.);
#3361=ORIENTED_EDGE('',*,*,#2496,.T.);
#3362=ORIENTED_EDGE('',*,*,#2494,.T.);
#3363=ORIENTED_EDGE('',*,*,#2496,.F.);
#3364=ORIENTED_EDGE('',*,*,#2497,.F.);
#3365=ORIENTED_EDGE('',*,*,#2495,.T.);
#3366=ORIENTED_EDGE('',*,*,#2498,.F.);
#3367=ORIENTED_EDGE('',*,*,#2499,.T.);
#3368=ORIENTED_EDGE('',*,*,#2497,.T.);
#3369=ORIENTED_EDGE('',*,*,#2499,.F.);
#3370=ORIENTED_EDGE('',*,*,#2498,.T.);
#3371=ORIENTED_EDGE('',*,*,#2500,.F.);
#3372=ORIENTED_EDGE('',*,*,#2501,.F.);
#3373=ORIENTED_EDGE('',*,*,#2502,.T.);
#3374=ORIENTED_EDGE('',*,*,#2500,.T.);
#3375=ORIENTED_EDGE('',*,*,#2502,.F.);
#3376=ORIENTED_EDGE('',*,*,#2503,.F.);
#3377=ORIENTED_EDGE('',*,*,#2501,.T.);
#3378=ORIENTED_EDGE('',*,*,#2504,.F.);
#3379=ORIENTED_EDGE('',*,*,#2505,.T.);
#3380=ORIENTED_EDGE('',*,*,#2503,.T.);
#3381=ORIENTED_EDGE('',*,*,#2505,.F.);
#3382=ORIENTED_EDGE('',*,*,#2504,.T.);
#3383=ORIENTED_EDGE('',*,*,#2506,.F.);
#3384=ORIENTED_EDGE('',*,*,#2506,.T.);
#3385=ORIENTED_EDGE('',*,*,#2507,.T.);
#3386=ORIENTED_EDGE('',*,*,#2491,.F.);
#3387=ORIENTED_EDGE('',*,*,#2507,.F.);
#3388=ORIENTED_EDGE('',*,*,#2485,.T.);
#3389=ORIENTED_EDGE('',*,*,#2488,.T.);
#3390=ORIENTED_EDGE('',*,*,#2478,.T.);
#3391=ORIENTED_EDGE('',*,*,#2482,.T.);
#3392=ORIENTED_EDGE('',*,*,#2508,.F.);
#3393=ORIENTED_EDGE('',*,*,#2509,.F.);
#3394=ORIENTED_EDGE('',*,*,#2510,.F.);
#3395=ORIENTED_EDGE('',*,*,#2511,.F.);
#3396=ORIENTED_EDGE('',*,*,#2512,.F.);
#3397=ORIENTED_EDGE('',*,*,#2511,.T.);
#3398=ORIENTED_EDGE('',*,*,#2513,.F.);
#3399=ORIENTED_EDGE('',*,*,#2514,.T.);
#3400=ORIENTED_EDGE('',*,*,#2515,.F.);
#3401=ORIENTED_EDGE('',*,*,#2514,.F.);
#3402=ORIENTED_EDGE('',*,*,#2516,.F.);
#3403=ORIENTED_EDGE('',*,*,#2517,.F.);
#3404=ORIENTED_EDGE('',*,*,#2518,.F.);
#3405=ORIENTED_EDGE('',*,*,#2517,.T.);
#3406=ORIENTED_EDGE('',*,*,#2519,.F.);
#3407=ORIENTED_EDGE('',*,*,#2509,.T.);
#3408=ORIENTED_EDGE('',*,*,#2520,.F.);
#3409=ORIENTED_EDGE('',*,*,#2521,.T.);
#3410=ORIENTED_EDGE('',*,*,#2522,.F.);
#3411=ORIENTED_EDGE('',*,*,#2523,.T.);
#3412=ORIENTED_EDGE('',*,*,#2520,.T.);
#3413=ORIENTED_EDGE('',*,*,#2523,.F.);
#3414=ORIENTED_EDGE('',*,*,#2515,.T.);
#3415=ORIENTED_EDGE('',*,*,#2518,.T.);
#3416=ORIENTED_EDGE('',*,*,#2508,.T.);
#3417=ORIENTED_EDGE('',*,*,#2512,.T.);
#3418=ORIENTED_EDGE('',*,*,#2522,.T.);
#3419=ORIENTED_EDGE('',*,*,#2524,.F.);
#3420=ORIENTED_EDGE('',*,*,#2524,.T.);
#3421=ORIENTED_EDGE('',*,*,#2525,.T.);
#3422=ORIENTED_EDGE('',*,*,#2521,.F.);
#3423=ORIENTED_EDGE('',*,*,#2525,.F.);
#3424=ORIENTED_EDGE('',*,*,#2516,.T.);
#3425=ORIENTED_EDGE('',*,*,#2513,.T.);
#3426=ORIENTED_EDGE('',*,*,#2510,.T.);
#3427=ORIENTED_EDGE('',*,*,#2519,.T.);
#3428=ORIENTED_EDGE('',*,*,#2526,.F.);
#3429=ORIENTED_EDGE('',*,*,#2527,.T.);
#3430=ORIENTED_EDGE('',*,*,#2528,.F.);
#3431=ORIENTED_EDGE('',*,*,#2529,.F.);
#3432=ORIENTED_EDGE('',*,*,#2530,.F.);
#3433=ORIENTED_EDGE('',*,*,#2531,.F.);
#3434=ORIENTED_EDGE('',*,*,#2527,.F.);
#3435=ORIENTED_EDGE('',*,*,#2532,.F.);
#3436=ORIENTED_EDGE('',*,*,#2533,.T.);
#3437=ORIENTED_EDGE('',*,*,#2534,.F.);
#3438=ORIENTED_EDGE('',*,*,#2535,.F.);
#3439=ORIENTED_EDGE('',*,*,#2536,.F.);
#3440=ORIENTED_EDGE('',*,*,#2533,.F.);
#3441=ORIENTED_EDGE('',*,*,#2537,.F.);
#3442=ORIENTED_EDGE('',*,*,#2529,.T.);
#3443=ORIENTED_EDGE('',*,*,#2538,.F.);
#3444=ORIENTED_EDGE('',*,*,#2539,.T.);
#3445=ORIENTED_EDGE('',*,*,#2530,.T.);
#3446=ORIENTED_EDGE('',*,*,#2537,.T.);
#3447=ORIENTED_EDGE('',*,*,#2528,.T.);
#3448=ORIENTED_EDGE('',*,*,#2540,.T.);
#3449=ORIENTED_EDGE('',*,*,#2541,.T.);
#3450=ORIENTED_EDGE('',*,*,#2540,.F.);
#3451=ORIENTED_EDGE('',*,*,#2532,.T.);
#3452=ORIENTED_EDGE('',*,*,#2526,.T.);
#3453=ORIENTED_EDGE('',*,*,#2531,.T.);
#3454=ORIENTED_EDGE('',*,*,#2539,.F.);
#3455=ORIENTED_EDGE('',*,*,#2542,.F.);
#3456=ORIENTED_EDGE('',*,*,#2543,.T.);
#3457=ORIENTED_EDGE('',*,*,#2535,.T.);
#3458=ORIENTED_EDGE('',*,*,#2534,.T.);
#3459=ORIENTED_EDGE('',*,*,#2544,.T.);
#3460=ORIENTED_EDGE('',*,*,#2545,.T.);
#3461=ORIENTED_EDGE('',*,*,#2544,.F.);
#3462=ORIENTED_EDGE('',*,*,#2536,.T.);
#3463=ORIENTED_EDGE('',*,*,#2543,.F.);
#3464=ORIENTED_EDGE('',*,*,#2542,.T.);
#3465=ORIENTED_EDGE('',*,*,#2538,.T.);
#3466=ORIENTED_EDGE('',*,*,#2545,.F.);
#3467=ORIENTED_EDGE('',*,*,#2541,.F.);
#3468=ORIENTED_EDGE('',*,*,#2546,.F.);
#3469=ORIENTED_EDGE('',*,*,#2547,.T.);
#3470=ORIENTED_EDGE('',*,*,#2548,.F.);
#3471=ORIENTED_EDGE('',*,*,#2549,.F.);
#3472=ORIENTED_EDGE('',*,*,#2550,.F.);
#3473=ORIENTED_EDGE('',*,*,#2551,.F.);
#3474=ORIENTED_EDGE('',*,*,#2547,.F.);
#3475=ORIENTED_EDGE('',*,*,#2552,.F.);
#3476=ORIENTED_EDGE('',*,*,#2553,.T.);
#3477=ORIENTED_EDGE('',*,*,#2554,.F.);
#3478=ORIENTED_EDGE('',*,*,#2555,.F.);
#3479=ORIENTED_EDGE('',*,*,#2556,.F.);
#3480=ORIENTED_EDGE('',*,*,#2553,.F.);
#3481=ORIENTED_EDGE('',*,*,#2557,.F.);
#3482=ORIENTED_EDGE('',*,*,#2549,.T.);
#3483=ORIENTED_EDGE('',*,*,#2558,.F.);
#3484=ORIENTED_EDGE('',*,*,#2559,.T.);
#3485=ORIENTED_EDGE('',*,*,#2550,.T.);
#3486=ORIENTED_EDGE('',*,*,#2557,.T.);
#3487=ORIENTED_EDGE('',*,*,#2548,.T.);
#3488=ORIENTED_EDGE('',*,*,#2560,.T.);
#3489=ORIENTED_EDGE('',*,*,#2561,.T.);
#3490=ORIENTED_EDGE('',*,*,#2560,.F.);
#3491=ORIENTED_EDGE('',*,*,#2552,.T.);
#3492=ORIENTED_EDGE('',*,*,#2546,.T.);
#3493=ORIENTED_EDGE('',*,*,#2551,.T.);
#3494=ORIENTED_EDGE('',*,*,#2559,.F.);
#3495=ORIENTED_EDGE('',*,*,#2562,.F.);
#3496=ORIENTED_EDGE('',*,*,#2563,.T.);
#3497=ORIENTED_EDGE('',*,*,#2555,.T.);
#3498=ORIENTED_EDGE('',*,*,#2554,.T.);
#3499=ORIENTED_EDGE('',*,*,#2564,.T.);
#3500=ORIENTED_EDGE('',*,*,#2565,.T.);
#3501=ORIENTED_EDGE('',*,*,#2564,.F.);
#3502=ORIENTED_EDGE('',*,*,#2556,.T.);
#3503=ORIENTED_EDGE('',*,*,#2563,.F.);
#3504=ORIENTED_EDGE('',*,*,#2562,.T.);
#3505=ORIENTED_EDGE('',*,*,#2558,.T.);
#3506=ORIENTED_EDGE('',*,*,#2565,.F.);
#3507=ORIENTED_EDGE('',*,*,#2561,.F.);
#3508=ORIENTED_EDGE('',*,*,#2566,.F.);
#3509=ORIENTED_EDGE('',*,*,#2567,.T.);
#3510=ORIENTED_EDGE('',*,*,#2568,.F.);
#3511=ORIENTED_EDGE('',*,*,#2567,.F.);
#3512=ORIENTED_EDGE('',*,*,#2566,.T.);
#3513=ORIENTED_EDGE('',*,*,#2569,.F.);
#3514=ORIENTED_EDGE('',*,*,#2569,.T.);
#3515=ORIENTED_EDGE('',*,*,#2570,.T.);
#3516=ORIENTED_EDGE('',*,*,#2571,.T.);
#3517=ORIENTED_EDGE('',*,*,#2570,.F.);
#3518=ORIENTED_EDGE('',*,*,#2572,.F.);
#3519=ORIENTED_EDGE('',*,*,#2573,.T.);
#3520=ORIENTED_EDGE('',*,*,#2574,.T.);
#3521=ORIENTED_EDGE('',*,*,#2573,.F.);
#3522=ORIENTED_EDGE('',*,*,#2572,.T.);
#3523=ORIENTED_EDGE('',*,*,#2568,.T.);
#3524=ORIENTED_EDGE('',*,*,#2574,.F.);
#3525=ORIENTED_EDGE('',*,*,#2571,.F.);
#3526=ORIENTED_EDGE('',*,*,#2575,.F.);
#3527=ORIENTED_EDGE('',*,*,#2576,.T.);
#3528=ORIENTED_EDGE('',*,*,#2577,.F.);
#3529=ORIENTED_EDGE('',*,*,#2576,.F.);
#3530=ORIENTED_EDGE('',*,*,#2575,.T.);
#3531=ORIENTED_EDGE('',*,*,#2578,.T.);
#3532=ORIENTED_EDGE('',*,*,#2579,.T.);
#3533=ORIENTED_EDGE('',*,*,#2580,.T.);
#3534=ORIENTED_EDGE('',*,*,#2579,.F.);
#3535=ORIENTED_EDGE('',*,*,#2581,.F.);
#3536=ORIENTED_EDGE('',*,*,#2582,.T.);
#3537=ORIENTED_EDGE('',*,*,#2578,.F.);
#3538=ORIENTED_EDGE('',*,*,#2582,.F.);
#3539=ORIENTED_EDGE('',*,*,#2580,.F.);
#3540=ORIENTED_EDGE('',*,*,#2583,.T.);
#3541=ORIENTED_EDGE('',*,*,#2584,.T.);
#3542=ORIENTED_EDGE('',*,*,#2581,.T.);
#3543=ORIENTED_EDGE('',*,*,#2584,.F.);
#3544=ORIENTED_EDGE('',*,*,#2583,.F.);
#3545=ORIENTED_EDGE('',*,*,#2577,.T.);
#3546=ORIENTED_EDGE('',*,*,#2585,.F.);
#3547=ORIENTED_EDGE('',*,*,#2586,.T.);
#3548=ORIENTED_EDGE('',*,*,#2587,.T.);
#3549=ORIENTED_EDGE('',*,*,#2588,.F.);
#3550=ORIENTED_EDGE('',*,*,#2589,.F.);
#3551=ORIENTED_EDGE('',*,*,#2590,.T.);
#3552=ORIENTED_EDGE('',*,*,#2591,.T.);
#3553=ORIENTED_EDGE('',*,*,#2586,.F.);
#3554=ORIENTED_EDGE('',*,*,#2592,.F.);
#3555=ORIENTED_EDGE('',*,*,#2593,.T.);
#3556=ORIENTED_EDGE('',*,*,#2594,.T.);
#3557=ORIENTED_EDGE('',*,*,#2590,.F.);
#3558=ORIENTED_EDGE('',*,*,#2595,.F.);
#3559=ORIENTED_EDGE('',*,*,#2596,.T.);
#3560=ORIENTED_EDGE('',*,*,#2597,.T.);
#3561=ORIENTED_EDGE('',*,*,#2593,.F.);
#3562=ORIENTED_EDGE('',*,*,#2598,.F.);
#3563=ORIENTED_EDGE('',*,*,#2599,.T.);
#3564=ORIENTED_EDGE('',*,*,#2600,.T.);
#3565=ORIENTED_EDGE('',*,*,#2596,.F.);
#3566=ORIENTED_EDGE('',*,*,#2601,.F.);
#3567=ORIENTED_EDGE('',*,*,#2588,.T.);
#3568=ORIENTED_EDGE('',*,*,#2602,.T.);
#3569=ORIENTED_EDGE('',*,*,#2599,.F.);
#3570=ORIENTED_EDGE('',*,*,#2602,.F.);
#3571=ORIENTED_EDGE('',*,*,#2587,.F.);
#3572=ORIENTED_EDGE('',*,*,#2591,.F.);
#3573=ORIENTED_EDGE('',*,*,#2594,.F.);
#3574=ORIENTED_EDGE('',*,*,#2597,.F.);
#3575=ORIENTED_EDGE('',*,*,#2600,.F.);
#3576=ORIENTED_EDGE('',*,*,#2603,.F.);
#3577=ORIENTED_EDGE('',*,*,#2585,.T.);
#3578=ORIENTED_EDGE('',*,*,#2601,.T.);
#3579=ORIENTED_EDGE('',*,*,#2598,.T.);
#3580=ORIENTED_EDGE('',*,*,#2595,.T.);
#3581=ORIENTED_EDGE('',*,*,#2592,.T.);
#3582=ORIENTED_EDGE('',*,*,#2589,.T.);
#3583=ORIENTED_EDGE('',*,*,#2604,.F.);
#3584=ORIENTED_EDGE('',*,*,#2605,.T.);
#3585=ORIENTED_EDGE('',*,*,#2603,.T.);
#3586=ORIENTED_EDGE('',*,*,#2605,.F.);
#3587=ORIENTED_EDGE('',*,*,#2606,.F.);
#3588=ORIENTED_EDGE('',*,*,#2607,.T.);
#3589=ORIENTED_EDGE('',*,*,#2604,.T.);
#3590=ORIENTED_EDGE('',*,*,#2607,.F.);
#3591=ORIENTED_EDGE('',*,*,#2608,.F.);
#3592=ORIENTED_EDGE('',*,*,#2609,.T.);
#3593=ORIENTED_EDGE('',*,*,#2606,.T.);
#3594=ORIENTED_EDGE('',*,*,#2609,.F.);
#3595=ORIENTED_EDGE('',*,*,#2608,.T.);
#3596=ORIENTED_EDGE('',*,*,#2610,.F.);
#3597=ORIENTED_EDGE('',*,*,#2611,.F.);
#3598=ORIENTED_EDGE('',*,*,#2612,.T.);
#3599=ORIENTED_EDGE('',*,*,#2610,.T.);
#3600=ORIENTED_EDGE('',*,*,#2612,.F.);
#3601=ORIENTED_EDGE('',*,*,#2613,.F.);
#3602=ORIENTED_EDGE('',*,*,#2614,.T.);
#3603=ORIENTED_EDGE('',*,*,#2611,.T.);
#3604=ORIENTED_EDGE('',*,*,#2614,.F.);
#3605=ORIENTED_EDGE('',*,*,#2615,.F.);
#3606=ORIENTED_EDGE('',*,*,#2616,.T.);
#3607=ORIENTED_EDGE('',*,*,#2613,.T.);
#3608=ORIENTED_EDGE('',*,*,#2616,.F.);
#3609=ORIENTED_EDGE('',*,*,#2615,.T.);
#3610=ORIENTED_EDGE('',*,*,#2617,.F.);
#3611=ORIENTED_EDGE('',*,*,#2618,.F.);
#3612=ORIENTED_EDGE('',*,*,#2619,.T.);
#3613=ORIENTED_EDGE('',*,*,#2617,.T.);
#3614=ORIENTED_EDGE('',*,*,#2619,.F.);
#3615=ORIENTED_EDGE('',*,*,#2620,.F.);
#3616=ORIENTED_EDGE('',*,*,#2621,.T.);
#3617=ORIENTED_EDGE('',*,*,#2618,.T.);
#3618=ORIENTED_EDGE('',*,*,#2621,.F.);
#3619=ORIENTED_EDGE('',*,*,#2622,.F.);
#3620=ORIENTED_EDGE('',*,*,#2623,.T.);
#3621=ORIENTED_EDGE('',*,*,#2620,.T.);
#3622=ORIENTED_EDGE('',*,*,#2623,.F.);
#3623=ORIENTED_EDGE('',*,*,#2622,.T.);
#3624=ORIENTED_EDGE('',*,*,#2624,.T.);
#3625=ORIENTED_EDGE('',*,*,#2625,.T.);
#3626=ORIENTED_EDGE('',*,*,#2626,.T.);
#3627=ORIENTED_EDGE('',*,*,#2627,.F.);
#3628=ORIENTED_EDGE('',*,*,#2628,.T.);
#3629=ORIENTED_EDGE('',*,*,#2629,.T.);
#3630=ORIENTED_EDGE('',*,*,#2630,.T.);
#3631=ORIENTED_EDGE('',*,*,#2625,.F.);
#3632=ORIENTED_EDGE('',*,*,#2631,.T.);
#3633=ORIENTED_EDGE('',*,*,#2632,.T.);
#3634=ORIENTED_EDGE('',*,*,#2633,.T.);
#3635=ORIENTED_EDGE('',*,*,#2629,.F.);
#3636=ORIENTED_EDGE('',*,*,#2634,.T.);
#3637=ORIENTED_EDGE('',*,*,#2635,.T.);
#3638=ORIENTED_EDGE('',*,*,#2636,.T.);
#3639=ORIENTED_EDGE('',*,*,#2632,.F.);
#3640=ORIENTED_EDGE('',*,*,#2637,.T.);
#3641=ORIENTED_EDGE('',*,*,#2638,.T.);
#3642=ORIENTED_EDGE('',*,*,#2639,.T.);
#3643=ORIENTED_EDGE('',*,*,#2635,.F.);
#3644=ORIENTED_EDGE('',*,*,#2640,.T.);
#3645=ORIENTED_EDGE('',*,*,#2627,.T.);
#3646=ORIENTED_EDGE('',*,*,#2641,.T.);
#3647=ORIENTED_EDGE('',*,*,#2638,.F.);
#3648=ORIENTED_EDGE('',*,*,#2640,.F.);
#3649=ORIENTED_EDGE('',*,*,#2637,.F.);
#3650=ORIENTED_EDGE('',*,*,#2634,.F.);
#3651=ORIENTED_EDGE('',*,*,#2631,.F.);
#3652=ORIENTED_EDGE('',*,*,#2628,.F.);
#3653=ORIENTED_EDGE('',*,*,#2624,.F.);
#3654=ORIENTED_EDGE('',*,*,#2641,.F.);
#3655=ORIENTED_EDGE('',*,*,#2626,.F.);
#3656=ORIENTED_EDGE('',*,*,#2630,.F.);
#3657=ORIENTED_EDGE('',*,*,#2633,.F.);
#3658=ORIENTED_EDGE('',*,*,#2636,.F.);
#3659=ORIENTED_EDGE('',*,*,#2639,.F.);
#3660=CYLINDRICAL_SURFACE('',#4210,0.274999999999999);
#3661=CYLINDRICAL_SURFACE('',#4213,0.275);
#3662=CYLINDRICAL_SURFACE('',#4216,0.275);
#3663=CYLINDRICAL_SURFACE('',#4219,0.274999999999999);
#3664=CYLINDRICAL_SURFACE('',#4229,0.165);
#3665=CYLINDRICAL_SURFACE('',#4237,0.165);
#3666=CYLINDRICAL_SURFACE('',#4244,0.165);
#3667=CYLINDRICAL_SURFACE('',#4260,0.165);
#3668=CYLINDRICAL_SURFACE('',#4267,0.165);
#3669=CYLINDRICAL_SURFACE('',#4274,0.165);
#3670=CYLINDRICAL_SURFACE('',#4278,1.6);
#3671=CYLINDRICAL_SURFACE('',#4282,2.);
#3672=CYLINDRICAL_SURFACE('',#4286,2.);
#3673=CYLINDRICAL_SURFACE('',#4288,1.05);
#3674=CYLINDRICAL_SURFACE('',#4294,0.21);
#3675=CYLINDRICAL_SURFACE('',#4298,0.21);
#3676=CYLINDRICAL_SURFACE('',#4302,0.21);
#3677=CYLINDRICAL_SURFACE('',#4306,0.21);
#3678=CYLINDRICAL_SURFACE('',#4310,1.6);
#3679=CYLINDRICAL_SURFACE('',#4324,0.475);
#3680=CYLINDRICAL_SURFACE('',#4329,0.475);
#3681=CYLINDRICAL_SURFACE('',#4333,0.275);
#3682=CYLINDRICAL_SURFACE('',#4335,0.275);
#3683=CYLINDRICAL_SURFACE('',#4337,1.6);
#3684=CYLINDRICAL_SURFACE('',#4346,0.21);
#3685=CYLINDRICAL_SURFACE('',#4350,0.21);
#3686=CYLINDRICAL_SURFACE('',#4354,0.21);
#3687=CYLINDRICAL_SURFACE('',#4358,0.21);
#3688=CYLINDRICAL_SURFACE('',#4362,1.6);
#3689=CYLINDRICAL_SURFACE('',#4376,0.475000000000001);
#3690=CYLINDRICAL_SURFACE('',#4381,0.475000000000001);
#3691=CYLINDRICAL_SURFACE('',#4385,0.274999999999999);
#3692=CYLINDRICAL_SURFACE('',#4387,0.274999999999999);
#3693=CYLINDRICAL_SURFACE('',#4389,1.6);
#3694=CYLINDRICAL_SURFACE('',#4398,0.7);
#3695=CYLINDRICAL_SURFACE('',#4401,1.04);
#3696=CYLINDRICAL_SURFACE('',#4407,0.7);
#3697=CYLINDRICAL_SURFACE('',#4410,1.04);
#3698=CYLINDRICAL_SURFACE('',#4416,0.7);
#3699=CYLINDRICAL_SURFACE('',#4419,1.04);
#3700=CYLINDRICAL_SURFACE('',#4425,0.225);
#3701=CYLINDRICAL_SURFACE('',#4428,0.225);
#3702=CYLINDRICAL_SURFACE('',#4431,0.225);
#3703=CYLINDRICAL_SURFACE('',#4434,1.1);
#3704=CYLINDRICAL_SURFACE('',#4439,0.7);
#3705=CYLINDRICAL_SURFACE('',#4441,2.);
#3706=CYLINDRICAL_SURFACE('',#4449,0.225);
#3707=CYLINDRICAL_SURFACE('',#4451,0.164999999999999);
#3708=CYLINDRICAL_SURFACE('',#4456,0.225);
#3709=CYLINDRICAL_SURFACE('',#4463,0.225);
#3710=CYLINDRICAL_SURFACE('',#4470,0.225);
#3711=CYLINDRICAL_SURFACE('',#4474,1.5);
#3712=CYLINDRICAL_SURFACE('',#4488,0.61);
#3713=CYLINDRICAL_SURFACE('',#4490,2.);
#3714=CYLINDRICAL_SURFACE('',#4498,0.425);
#3715=CYLINDRICAL_SURFACE('',#4506,0.24505);
#3716=CYLINDRICAL_SURFACE('',#4531,1.05);
#3717=CYLINDRICAL_SURFACE('',#4535,1.);
#3718=CYLINDRICAL_SURFACE('',#4539,1.05);
#3719=CYLINDRICAL_SURFACE('',#4543,1.);
#3720=CYLINDRICAL_SURFACE('',#4547,1.05);
#3721=CYLINDRICAL_SURFACE('',#4551,0.9);
#3722=CYLINDRICAL_SURFACE('',#4564,0.895);
#3723=CYLINDRICAL_SURFACE('',#4568,0.605);
#3724=CYLINDRICAL_SURFACE('',#4575,0.210000000000001);
#3725=CYLINDRICAL_SURFACE('',#4578,0.605);
#3726=CYLINDRICAL_SURFACE('',#4581,1.1);
#3727=CYLINDRICAL_SURFACE('',#4589,0.210000000000001);
#3728=CYLINDRICAL_SURFACE('',#4592,0.605);
#3729=CYLINDRICAL_SURFACE('',#4595,1.1);
#3730=CYLINDRICAL_SURFACE('',#4601,0.375);
#3731=CYLINDRICAL_SURFACE('',#4606,0.225);
#3732=CYLINDRICAL_SURFACE('',#4608,1.4);
#3733=CYLINDRICAL_SURFACE('',#4614,0.165);
#3734=CYLINDRICAL_SURFACE('',#4621,0.6);
#3735=CYLINDRICAL_SURFACE('',#4639,0.24505);
#3736=CYLINDRICAL_SURFACE('',#4649,0.35);
#3737=CYLINDRICAL_SURFACE('',#4657,0.1954);
#3738=ADVANCED_FACE('',(#495),#3660,.F.);
#3739=ADVANCED_FACE('',(#496),#3661,.F.);
#3740=ADVANCED_FACE('',(#497),#3662,.F.);
#3741=ADVANCED_FACE('',(#498),#3663,.F.);
#3742=ADVANCED_FACE('',(#499),#359,.T.);
#3743=ADVANCED_FACE('',(#500),#360,.T.);
#3744=ADVANCED_FACE('',(#501),#361,.T.);
#3745=ADVANCED_FACE('',(#502),#362,.T.);
#3746=ADVANCED_FACE('',(#503,#279,#280,#281,#282),#363,.T.);
#3747=ADVANCED_FACE('',(#504,#283,#284,#285,#286),#364,.F.);
#3748=ADVANCED_FACE('',(#505),#3664,.F.);
#3749=ADVANCED_FACE('',(#506),#365,.T.);
#3750=ADVANCED_FACE('',(#507),#3665,.F.);
#3751=ADVANCED_FACE('',(#508),#366,.T.);
#3752=ADVANCED_FACE('',(#509),#3666,.F.);
#3753=ADVANCED_FACE('',(#510),#367,.T.);
#3754=ADVANCED_FACE('',(#511,#287),#368,.F.);
#3755=ADVANCED_FACE('',(#512),#369,.F.);
#3756=ADVANCED_FACE('',(#513),#3667,.F.);
#3757=ADVANCED_FACE('',(#514),#370,.F.);
#3758=ADVANCED_FACE('',(#515),#3668,.F.);
#3759=ADVANCED_FACE('',(#516),#371,.F.);
#3760=ADVANCED_FACE('',(#517),#3669,.F.);
#3761=ADVANCED_FACE('',(#518),#3670,.T.);
#3762=ADVANCED_FACE('',(#519),#3671,.T.);
#3763=ADVANCED_FACE('',(#520,#288),#372,.T.);
#3764=ADVANCED_FACE('',(#521),#3672,.T.);
#3765=ADVANCED_FACE('',(#522),#3673,.F.);
#3766=ADVANCED_FACE('',(#523,#289,#290,#291,#292),#373,.T.);
#3767=ADVANCED_FACE('',(#524,#293,#294,#295,#296),#374,.F.);
#3768=ADVANCED_FACE('',(#525),#3674,.F.);
#3769=ADVANCED_FACE('',(#526),#375,.T.);
#3770=ADVANCED_FACE('',(#527),#3675,.F.);
#3771=ADVANCED_FACE('',(#528),#376,.T.);
#3772=ADVANCED_FACE('',(#529),#3676,.F.);
#3773=ADVANCED_FACE('',(#530),#377,.F.);
#3774=ADVANCED_FACE('',(#531),#3677,.F.);
#3775=ADVANCED_FACE('',(#532),#378,.F.);
#3776=ADVANCED_FACE('',(#533),#3678,.F.);
#3777=ADVANCED_FACE('',(#534),#379,.T.);
#3778=ADVANCED_FACE('',(#535,#297),#380,.T.);
#3779=ADVANCED_FACE('',(#536),#381,.T.);
#3780=ADVANCED_FACE('',(#537),#382,.T.);
#3781=ADVANCED_FACE('',(#538),#383,.T.);
#3782=ADVANCED_FACE('',(#539,#298),#384,.T.);
#3783=ADVANCED_FACE('',(#540,#299,#300),#385,.F.);
#3784=ADVANCED_FACE('',(#541,#301),#386,.T.);
#3785=ADVANCED_FACE('',(#542),#3679,.F.);
#3786=ADVANCED_FACE('',(#543,#302),#387,.T.);
#3787=ADVANCED_FACE('',(#544),#3680,.F.);
#3788=ADVANCED_FACE('',(#545),#388,.T.);
#3789=ADVANCED_FACE('',(#546),#389,.T.);
#3790=ADVANCED_FACE('',(#547),#3681,.F.);
#3791=ADVANCED_FACE('',(#548),#3682,.F.);
#3792=ADVANCED_FACE('',(#549),#3683,.F.);
#3793=ADVANCED_FACE('',(#550),#390,.T.);
#3794=ADVANCED_FACE('',(#551,#303),#391,.F.);
#3795=ADVANCED_FACE('',(#552),#392,.T.);
#3796=ADVANCED_FACE('',(#553),#393,.T.);
#3797=ADVANCED_FACE('',(#554,#304),#394,.F.);
#3798=ADVANCED_FACE('',(#555),#3684,.F.);
#3799=ADVANCED_FACE('',(#556),#395,.T.);
#3800=ADVANCED_FACE('',(#557),#3685,.F.);
#3801=ADVANCED_FACE('',(#558),#396,.T.);
#3802=ADVANCED_FACE('',(#559),#3686,.F.);
#3803=ADVANCED_FACE('',(#560),#397,.F.);
#3804=ADVANCED_FACE('',(#561),#3687,.F.);
#3805=ADVANCED_FACE('',(#562),#398,.F.);
#3806=ADVANCED_FACE('',(#563),#3688,.F.);
#3807=ADVANCED_FACE('',(#564),#399,.T.);
#3808=ADVANCED_FACE('',(#565,#305),#400,.T.);
#3809=ADVANCED_FACE('',(#566),#401,.T.);
#3810=ADVANCED_FACE('',(#567),#402,.T.);
#3811=ADVANCED_FACE('',(#568),#403,.T.);
#3812=ADVANCED_FACE('',(#569,#306),#404,.T.);
#3813=ADVANCED_FACE('',(#570,#307,#308),#405,.F.);
#3814=ADVANCED_FACE('',(#571,#309),#406,.T.);
#3815=ADVANCED_FACE('',(#572),#3689,.F.);
#3816=ADVANCED_FACE('',(#573,#310),#407,.T.);
#3817=ADVANCED_FACE('',(#574),#3690,.F.);
#3818=ADVANCED_FACE('',(#575),#408,.T.);
#3819=ADVANCED_FACE('',(#576),#409,.T.);
#3820=ADVANCED_FACE('',(#577),#3691,.F.);
#3821=ADVANCED_FACE('',(#578),#3692,.F.);
#3822=ADVANCED_FACE('',(#579),#3693,.F.);
#3823=ADVANCED_FACE('',(#580),#410,.T.);
#3824=ADVANCED_FACE('',(#581,#311),#411,.F.);
#3825=ADVANCED_FACE('',(#582),#412,.T.);
#3826=ADVANCED_FACE('',(#583),#413,.T.);
#3827=ADVANCED_FACE('',(#584,#312),#414,.F.);
#3828=ADVANCED_FACE('',(#585),#3694,.F.);
#3829=ADVANCED_FACE('',(#586),#3695,.T.);
#3830=ADVANCED_FACE('',(#587,#313),#415,.T.);
#3831=ADVANCED_FACE('',(#588,#314),#416,.F.);
#3832=ADVANCED_FACE('',(#589),#3696,.F.);
#3833=ADVANCED_FACE('',(#590),#3697,.T.);
#3834=ADVANCED_FACE('',(#591,#315),#417,.T.);
#3835=ADVANCED_FACE('',(#592,#316),#418,.F.);
#3836=ADVANCED_FACE('',(#593),#3698,.F.);
#3837=ADVANCED_FACE('',(#594),#3699,.T.);
#3838=ADVANCED_FACE('',(#595,#317),#419,.T.);
#3839=ADVANCED_FACE('',(#596,#318),#420,.F.);
#3840=ADVANCED_FACE('',(#597),#3700,.F.);
#3841=ADVANCED_FACE('',(#598),#3701,.F.);
#3842=ADVANCED_FACE('',(#599),#3702,.F.);
#3843=ADVANCED_FACE('',(#600),#3703,.T.);
#3844=ADVANCED_FACE('',(#601,#319),#421,.F.);
#3845=ADVANCED_FACE('',(#602),#3704,.F.);
#3846=ADVANCED_FACE('',(#603),#3705,.T.);
#3847=ADVANCED_FACE('',(#604,#320,#321,#322,#323),#422,.T.);
#3848=ADVANCED_FACE('',(#605,#324,#325,#326,#327),#423,.F.);
#3849=ADVANCED_FACE('',(#606),#424,.F.);
#3850=ADVANCED_FACE('',(#607),#3706,.F.);
#3851=ADVANCED_FACE('',(#608),#3707,.F.);
#3852=ADVANCED_FACE('',(#609),#425,.F.);
#3853=ADVANCED_FACE('',(#610),#3708,.F.);
#3854=ADVANCED_FACE('',(#611),#426,.F.);
#3855=ADVANCED_FACE('',(#612),#3709,.F.);
#3856=ADVANCED_FACE('',(#613),#427,.F.);
#3857=ADVANCED_FACE('',(#614),#3710,.F.);
#3858=ADVANCED_FACE('',(#615,#328,#329),#3711,.T.);
#3859=ADVANCED_FACE('',(#616,#330),#428,.F.);
#3860=ADVANCED_FACE('',(#617,#331),#429,.F.);
#3861=ADVANCED_FACE('',(#618,#332),#430,.T.);
#3862=ADVANCED_FACE('',(#619),#431,.T.);
#3863=ADVANCED_FACE('',(#620),#3712,.F.);
#3864=ADVANCED_FACE('',(#621),#3713,.T.);
#3865=ADVANCED_FACE('',(#622,#333,#334,#335,#336),#432,.F.);
#3866=ADVANCED_FACE('',(#623),#433,.T.);
#3867=ADVANCED_FACE('',(#624),#169,.T.);
#3868=ADVANCED_FACE('',(#625),#3714,.T.);
#3869=ADVANCED_FACE('',(#626),#170,.T.);
#3870=ADVANCED_FACE('',(#627,#337),#434,.T.);
#3871=ADVANCED_FACE('',(#628),#171,.T.);
#3872=ADVANCED_FACE('',(#629),#3715,.T.);
#3873=ADVANCED_FACE('',(#630),#172,.T.);
#3874=ADVANCED_FACE('',(#631),#435,.T.);
#3875=ADVANCED_FACE('',(#632),#436,.F.);
#3876=ADVANCED_FACE('',(#633),#437,.F.);
#3877=ADVANCED_FACE('',(#634),#438,.F.);
#3878=ADVANCED_FACE('',(#635),#439,.F.);
#3879=ADVANCED_FACE('',(#636),#440,.F.);
#3880=ADVANCED_FACE('',(#637),#441,.F.);
#3881=ADVANCED_FACE('',(#638),#442,.F.);
#3882=ADVANCED_FACE('',(#639),#443,.F.);
#3883=ADVANCED_FACE('',(#640),#444,.F.);
#3884=ADVANCED_FACE('',(#641),#445,.F.);
#3885=ADVANCED_FACE('',(#642),#446,.F.);
#3886=ADVANCED_FACE('',(#643),#447,.F.);
#3887=ADVANCED_FACE('',(#644),#448,.F.);
#3888=ADVANCED_FACE('',(#645,#338),#449,.T.);
#3889=ADVANCED_FACE('',(#646),#3716,.T.);
#3890=ADVANCED_FACE('',(#647,#339),#450,.T.);
#3891=ADVANCED_FACE('',(#648),#3717,.T.);
#3892=ADVANCED_FACE('',(#649,#340),#451,.T.);
#3893=ADVANCED_FACE('',(#650),#3718,.T.);
#3894=ADVANCED_FACE('',(#651,#341),#452,.T.);
#3895=ADVANCED_FACE('',(#652),#3719,.T.);
#3896=ADVANCED_FACE('',(#653,#342),#453,.T.);
#3897=ADVANCED_FACE('',(#654),#3720,.T.);
#3898=ADVANCED_FACE('',(#655,#343),#454,.T.);
#3899=ADVANCED_FACE('',(#656,#344),#3721,.F.);
#3900=ADVANCED_FACE('',(#657),#455,.F.);
#3901=ADVANCED_FACE('',(#658),#456,.F.);
#3902=ADVANCED_FACE('',(#659),#457,.F.);
#3903=ADVANCED_FACE('',(#660),#458,.F.);
#3904=ADVANCED_FACE('',(#661,#345),#459,.T.);
#3905=ADVANCED_FACE('',(#662,#346),#3722,.T.);
#3906=ADVANCED_FACE('',(#663,#347),#460,.T.);
#3907=ADVANCED_FACE('',(#664,#348),#3723,.F.);
#3908=ADVANCED_FACE('',(#665),#461,.T.);
#3909=ADVANCED_FACE('',(#666),#3724,.F.);
#3910=ADVANCED_FACE('',(#667),#462,.T.);
#3911=ADVANCED_FACE('',(#668),#3725,.F.);
#3912=ADVANCED_FACE('',(#669),#3726,.T.);
#3913=ADVANCED_FACE('',(#670,#349),#463,.T.);
#3914=ADVANCED_FACE('',(#671,#350),#464,.F.);
#3915=ADVANCED_FACE('',(#672),#465,.T.);
#3916=ADVANCED_FACE('',(#673),#3727,.F.);
#3917=ADVANCED_FACE('',(#674),#466,.T.);
#3918=ADVANCED_FACE('',(#675),#3728,.F.);
#3919=ADVANCED_FACE('',(#676),#3729,.T.);
#3920=ADVANCED_FACE('',(#677,#351),#467,.T.);
#3921=ADVANCED_FACE('',(#678,#352),#468,.F.);
#3922=ADVANCED_FACE('',(#679),#3730,.F.);
#3923=ADVANCED_FACE('',(#680,#353),#469,.T.);
#3924=ADVANCED_FACE('',(#681),#3731,.F.);
#3925=ADVANCED_FACE('',(#682),#3732,.T.);
#3926=ADVANCED_FACE('',(#683,#354),#470,.T.);
#3927=ADVANCED_FACE('',(#684,#355),#471,.F.);
#3928=ADVANCED_FACE('',(#685),#3733,.F.);
#3929=ADVANCED_FACE('',(#686),#472,.T.);
#3930=ADVANCED_FACE('',(#687),#173,.T.);
#3931=ADVANCED_FACE('',(#688),#3734,.T.);
#3932=ADVANCED_FACE('',(#689),#473,.F.);
#3933=ADVANCED_FACE('',(#690),#174,.T.);
#3934=ADVANCED_FACE('',(#691,#356),#474,.T.);
#3935=ADVANCED_FACE('',(#692),#475,.F.);
#3936=ADVANCED_FACE('',(#693),#476,.F.);
#3937=ADVANCED_FACE('',(#694),#477,.F.);
#3938=ADVANCED_FACE('',(#695),#478,.F.);
#3939=ADVANCED_FACE('',(#696),#479,.F.);
#3940=ADVANCED_FACE('',(#697),#480,.F.);
#3941=ADVANCED_FACE('',(#698),#481,.F.);
#3942=ADVANCED_FACE('',(#699,#357),#482,.T.);
#3943=ADVANCED_FACE('',(#700),#175,.T.);
#3944=ADVANCED_FACE('',(#701),#3735,.T.);
#3945=ADVANCED_FACE('',(#702),#176,.T.);
#3946=ADVANCED_FACE('',(#703),#483,.T.);
#3947=ADVANCED_FACE('',(#704),#484,.T.);
#3948=ADVANCED_FACE('',(#705),#177,.T.);
#3949=ADVANCED_FACE('',(#706),#3736,.T.);
#3950=ADVANCED_FACE('',(#707),#178,.T.);
#3951=ADVANCED_FACE('',(#708,#358),#485,.T.);
#3952=ADVANCED_FACE('',(#709),#179,.T.);
#3953=ADVANCED_FACE('',(#710),#3737,.T.);
#3954=ADVANCED_FACE('',(#711),#180,.T.);
#3955=ADVANCED_FACE('',(#712),#486,.T.);
#3956=ADVANCED_FACE('',(#713),#487,.F.);
#3957=ADVANCED_FACE('',(#714),#488,.F.);
#3958=ADVANCED_FACE('',(#715),#489,.F.);
#3959=ADVANCED_FACE('',(#716),#490,.F.);
#3960=ADVANCED_FACE('',(#717),#491,.F.);
#3961=ADVANCED_FACE('',(#718),#492,.F.);
#3962=ADVANCED_FACE('',(#719),#493,.F.);
#3963=ADVANCED_FACE('',(#720),#494,.F.);
#3964=CLOSED_SHELL('',(#3738,#3739,#3740,#3741,#3742,#3743,#3744,#3745,
#3746,#3747));
#3965=CLOSED_SHELL('',(#3748,#3749,#3750,#3751,#3752,#3753,#3754,#3755,
#3756,#3757,#3758,#3759,#3760,#3761,#3762,#3763,#3764,#3765,#3766,#3767));
#3966=CLOSED_SHELL('',(#3768,#3769,#3770,#3771,#3772,#3773,#3774,#3775,
#3776,#3777,#3778,#3779,#3780,#3781,#3782,#3783));
#3967=CLOSED_SHELL('',(#3784,#3785,#3786,#3787,#3788,#3789,#3790,#3791,
#3792,#3793,#3794,#3795,#3796,#3797));
#3968=CLOSED_SHELL('',(#3798,#3799,#3800,#3801,#3802,#3803,#3804,#3805,
#3806,#3807,#3808,#3809,#3810,#3811,#3812,#3813));
#3969=CLOSED_SHELL('',(#3814,#3815,#3816,#3817,#3818,#3819,#3820,#3821,
#3822,#3823,#3824,#3825,#3826,#3827));
#3970=CLOSED_SHELL('',(#3828,#3829,#3830,#3831));
#3971=CLOSED_SHELL('',(#3832,#3833,#3834,#3835));
#3972=CLOSED_SHELL('',(#3836,#3837,#3838,#3839));
#3973=CLOSED_SHELL('',(#3840,#3841,#3842,#3843,#3844,#3845,#3846,#3847,
#3848));
#3974=CLOSED_SHELL('',(#3849,#3850,#3851,#3852,#3853,#3854,#3855,#3856,
#3857,#3858,#3859,#3860,#3861,#3862,#3863,#3864,#3865));
#3975=CLOSED_SHELL('',(#3866,#3867,#3868,#3869,#3870,#3871,#3872,#3873,
#3874));
#3976=CLOSED_SHELL('',(#3875,#3876,#3877,#3878,#3879,#3880,#3881,#3882));
#3977=CLOSED_SHELL('',(#3883,#3884,#3885,#3886,#3887,#3888,#3889,#3890,
#3891,#3892,#3893,#3894,#3895,#3896,#3897,#3898,#3899));
#3978=CLOSED_SHELL('',(#3900,#3901,#3902,#3903,#3904,#3905,#3906,#3907));
#3979=CLOSED_SHELL('',(#3908,#3909,#3910,#3911,#3912,#3913,#3914));
#3980=CLOSED_SHELL('',(#3915,#3916,#3917,#3918,#3919,#3920,#3921));
#3981=CLOSED_SHELL('',(#3922,#3923,#3924,#3925,#3926,#3927));
#3982=CLOSED_SHELL('',(#3928,#3929,#3930,#3931,#3932,#3933,#3934));
#3983=CLOSED_SHELL('',(#3935,#3936,#3937,#3938,#3939,#3940,#3941,#3942,
#3943,#3944,#3945,#3946));
#3984=CLOSED_SHELL('',(#3947,#3948,#3949,#3950,#3951,#3952,#3953,#3954,
#3955));
#3985=CLOSED_SHELL('',(#3956,#3957,#3958,#3959,#3960,#3961,#3962,#3963));
#3986=DERIVED_UNIT_ELEMENT(#4026,1.);
#3987=DERIVED_UNIT_ELEMENT(#7351,-3.);
#3988=DERIVED_UNIT_ELEMENT(#4026,1.);
#3989=DERIVED_UNIT_ELEMENT(#7351,-3.);
#3990=DERIVED_UNIT_ELEMENT(#4026,1.);
#3991=DERIVED_UNIT_ELEMENT(#7351,-3.);
#3992=DERIVED_UNIT_ELEMENT(#4026,1.);
#3993=DERIVED_UNIT_ELEMENT(#7351,-3.);
#3994=DERIVED_UNIT_ELEMENT(#4026,1.);
#3995=DERIVED_UNIT_ELEMENT(#7351,-3.);
#3996=DERIVED_UNIT_ELEMENT(#4026,1.);
#3997=DERIVED_UNIT_ELEMENT(#7351,-3.);
#3998=DERIVED_UNIT_ELEMENT(#4026,1.);
#3999=DERIVED_UNIT_ELEMENT(#7351,-3.);
#4000=DERIVED_UNIT_ELEMENT(#4026,1.);
#4001=DERIVED_UNIT_ELEMENT(#7351,-3.);
#4002=DERIVED_UNIT_ELEMENT(#4026,1.);
#4003=DERIVED_UNIT_ELEMENT(#7351,-3.);
#4004=DERIVED_UNIT_ELEMENT(#4026,1.);
#4005=DERIVED_UNIT_ELEMENT(#7351,-3.);
#4006=DERIVED_UNIT_ELEMENT(#4026,1.);
#4007=DERIVED_UNIT_ELEMENT(#7351,-3.);
#4008=DERIVED_UNIT_ELEMENT(#4026,1.);
#4009=DERIVED_UNIT_ELEMENT(#7351,-3.);
#4010=DERIVED_UNIT_ELEMENT(#4026,1.);
#4011=DERIVED_UNIT_ELEMENT(#7351,-3.);
#4012=DERIVED_UNIT_ELEMENT(#4026,1.);
#4013=DERIVED_UNIT_ELEMENT(#7351,-3.);
#4014=DERIVED_UNIT_ELEMENT(#4026,1.);
#4015=DERIVED_UNIT_ELEMENT(#7351,-3.);
#4016=DERIVED_UNIT_ELEMENT(#4026,1.);
#4017=DERIVED_UNIT_ELEMENT(#7351,-3.);
#4018=DERIVED_UNIT_ELEMENT(#4026,1.);
#4019=DERIVED_UNIT_ELEMENT(#7351,-3.);
#4020=DERIVED_UNIT_ELEMENT(#4026,1.);
#4021=DERIVED_UNIT_ELEMENT(#7351,-3.);
#4022=DERIVED_UNIT_ELEMENT(#4026,1.);
#4023=DERIVED_UNIT_ELEMENT(#7351,-3.);
#4024=DERIVED_UNIT_ELEMENT(#4026,1.);
#4025=DERIVED_UNIT_ELEMENT(#7351,-3.);
#4026=(
MASS_UNIT()
NAMED_UNIT(*)
SI_UNIT(.KILO.,.GRAM.)
);
#4027=DERIVED_UNIT((#3986,#3987));
#4028=DERIVED_UNIT((#3988,#3989));
#4029=DERIVED_UNIT((#3990,#3991));
#4030=DERIVED_UNIT((#3992,#3993));
#4031=DERIVED_UNIT((#3994,#3995));
#4032=DERIVED_UNIT((#3996,#3997));
#4033=DERIVED_UNIT((#3998,#3999));
#4034=DERIVED_UNIT((#4000,#4001));
#4035=DERIVED_UNIT((#4002,#4003));
#4036=DERIVED_UNIT((#4004,#4005));
#4037=DERIVED_UNIT((#4006,#4007));
#4038=DERIVED_UNIT((#4008,#4009));
#4039=DERIVED_UNIT((#4010,#4011));
#4040=DERIVED_UNIT((#4012,#4013));
#4041=DERIVED_UNIT((#4014,#4015));
#4042=DERIVED_UNIT((#4016,#4017));
#4043=DERIVED_UNIT((#4018,#4019));
#4044=DERIVED_UNIT((#4020,#4021));
#4045=DERIVED_UNIT((#4022,#4023));
#4046=DERIVED_UNIT((#4024,#4025));
#4047=MEASURE_REPRESENTATION_ITEM('density measure',
POSITIVE_RATIO_MEASURE(7850.),#4027);
#4048=MEASURE_REPRESENTATION_ITEM('density measure',
POSITIVE_RATIO_MEASURE(7850.),#4028);
#4049=MEASURE_REPRESENTATION_ITEM('density measure',
POSITIVE_RATIO_MEASURE(7850.),#4029);
#4050=MEASURE_REPRESENTATION_ITEM('density measure',
POSITIVE_RATIO_MEASURE(7850.),#4030);
#4051=MEASURE_REPRESENTATION_ITEM('density measure',
POSITIVE_RATIO_MEASURE(7850.),#4031);
#4052=MEASURE_REPRESENTATION_ITEM('density measure',
POSITIVE_RATIO_MEASURE(7850.),#4032);
#4053=MEASURE_REPRESENTATION_ITEM('density measure',
POSITIVE_RATIO_MEASURE(7850.),#4033);
#4054=MEASURE_REPRESENTATION_ITEM('density measure',
POSITIVE_RATIO_MEASURE(7850.),#4034);
#4055=MEASURE_REPRESENTATION_ITEM('density measure',
POSITIVE_RATIO_MEASURE(7850.),#4035);
#4056=MEASURE_REPRESENTATION_ITEM('density measure',
POSITIVE_RATIO_MEASURE(7850.),#4036);
#4057=MEASURE_REPRESENTATION_ITEM('density measure',
POSITIVE_RATIO_MEASURE(7850.),#4037);
#4058=MEASURE_REPRESENTATION_ITEM('density measure',
POSITIVE_RATIO_MEASURE(7850.),#4038);
#4059=MEASURE_REPRESENTATION_ITEM('density measure',
POSITIVE_RATIO_MEASURE(7850.),#4039);
#4060=MEASURE_REPRESENTATION_ITEM('density measure',
POSITIVE_RATIO_MEASURE(7850.),#4040);
#4061=MEASURE_REPRESENTATION_ITEM('density measure',
POSITIVE_RATIO_MEASURE(7850.),#4041);
#4062=MEASURE_REPRESENTATION_ITEM('density measure',
POSITIVE_RATIO_MEASURE(7850.),#4042);
#4063=MEASURE_REPRESENTATION_ITEM('density measure',
POSITIVE_RATIO_MEASURE(7850.),#4043);
#4064=MEASURE_REPRESENTATION_ITEM('density measure',
POSITIVE_RATIO_MEASURE(7850.),#4044);
#4065=MEASURE_REPRESENTATION_ITEM('density measure',
POSITIVE_RATIO_MEASURE(7850.),#4045);
#4066=MEASURE_REPRESENTATION_ITEM('density measure',
POSITIVE_RATIO_MEASURE(7850.),#4046);
#4067=PROPERTY_DEFINITION_REPRESENTATION(#4167,#4107);
#4068=PROPERTY_DEFINITION_REPRESENTATION(#4168,#4108);
#4069=PROPERTY_DEFINITION_REPRESENTATION(#4169,#4109);
#4070=PROPERTY_DEFINITION_REPRESENTATION(#4170,#4110);
#4071=PROPERTY_DEFINITION_REPRESENTATION(#4171,#4111);
#4072=PROPERTY_DEFINITION_REPRESENTATION(#4172,#4112);
#4073=PROPERTY_DEFINITION_REPRESENTATION(#4173,#4113);
#4074=PROPERTY_DEFINITION_REPRESENTATION(#4174,#4114);
#4075=PROPERTY_DEFINITION_REPRESENTATION(#4175,#4115);
#4076=PROPERTY_DEFINITION_REPRESENTATION(#4176,#4116);
#4077=PROPERTY_DEFINITION_REPRESENTATION(#4177,#4117);
#4078=PROPERTY_DEFINITION_REPRESENTATION(#4178,#4118);
#4079=PROPERTY_DEFINITION_REPRESENTATION(#4179,#4119);
#4080=PROPERTY_DEFINITION_REPRESENTATION(#4180,#4120);
#4081=PROPERTY_DEFINITION_REPRESENTATION(#4181,#4121);
#4082=PROPERTY_DEFINITION_REPRESENTATION(#4182,#4122);
#4083=PROPERTY_DEFINITION_REPRESENTATION(#4183,#4123);
#4084=PROPERTY_DEFINITION_REPRESENTATION(#4184,#4124);
#4085=PROPERTY_DEFINITION_REPRESENTATION(#4185,#4125);
#4086=PROPERTY_DEFINITION_REPRESENTATION(#4186,#4126);
#4087=PROPERTY_DEFINITION_REPRESENTATION(#4187,#4127);
#4088=PROPERTY_DEFINITION_REPRESENTATION(#4188,#4128);
#4089=PROPERTY_DEFINITION_REPRESENTATION(#4189,#4129);
#4090=PROPERTY_DEFINITION_REPRESENTATION(#4190,#4130);
#4091=PROPERTY_DEFINITION_REPRESENTATION(#4191,#4131);
#4092=PROPERTY_DEFINITION_REPRESENTATION(#4192,#4132);
#4093=PROPERTY_DEFINITION_REPRESENTATION(#4193,#4133);
#4094=PROPERTY_DEFINITION_REPRESENTATION(#4194,#4134);
#4095=PROPERTY_DEFINITION_REPRESENTATION(#4195,#4135);
#4096=PROPERTY_DEFINITION_REPRESENTATION(#4196,#4136);
#4097=PROPERTY_DEFINITION_REPRESENTATION(#4197,#4137);
#4098=PROPERTY_DEFINITION_REPRESENTATION(#4198,#4138);
#4099=PROPERTY_DEFINITION_REPRESENTATION(#4199,#4139);
#4100=PROPERTY_DEFINITION_REPRESENTATION(#4200,#4140);
#4101=PROPERTY_DEFINITION_REPRESENTATION(#4201,#4141);
#4102=PROPERTY_DEFINITION_REPRESENTATION(#4202,#4142);
#4103=PROPERTY_DEFINITION_REPRESENTATION(#4203,#4143);
#4104=PROPERTY_DEFINITION_REPRESENTATION(#4204,#4144);
#4105=PROPERTY_DEFINITION_REPRESENTATION(#4205,#4145);
#4106=PROPERTY_DEFINITION_REPRESENTATION(#4206,#4146);
#4107=REPRESENTATION('material name',(#4147),#7327);
#4108=REPRESENTATION('density',(#4047),#7327);
#4109=REPRESENTATION('material name',(#4148),#7328);
#4110=REPRESENTATION('density',(#4048),#7328);
#4111=REPRESENTATION('material name',(#4149),#7329);
#4112=REPRESENTATION('density',(#4049),#7329);
#4113=REPRESENTATION('material name',(#4150),#7330);
#4114=REPRESENTATION('density',(#4050),#7330);
#4115=REPRESENTATION('material name',(#4151),#7331);
#4116=REPRESENTATION('density',(#4051),#7331);
#4117=REPRESENTATION('material name',(#4152),#7332);
#4118=REPRESENTATION('density',(#4052),#7332);
#4119=REPRESENTATION('material name',(#4153),#7333);
#4120=REPRESENTATION('density',(#4053),#7333);
#4121=REPRESENTATION('material name',(#4154),#7334);
#4122=REPRESENTATION('density',(#4054),#7334);
#4123=REPRESENTATION('material name',(#4155),#7335);
#4124=REPRESENTATION('density',(#4055),#7335);
#4125=REPRESENTATION('material name',(#4156),#7336);
#4126=REPRESENTATION('density',(#4056),#7336);
#4127=REPRESENTATION('material name',(#4157),#7337);
#4128=REPRESENTATION('density',(#4057),#7337);
#4129=REPRESENTATION('material name',(#4158),#7338);
#4130=REPRESENTATION('density',(#4058),#7338);
#4131=REPRESENTATION('material name',(#4159),#7340);
#4132=REPRESENTATION('density',(#4059),#7340);
#4133=REPRESENTATION('material name',(#4160),#7341);
#4134=REPRESENTATION('density',(#4060),#7341);
#4135=REPRESENTATION('material name',(#4161),#7343);
#4136=REPRESENTATION('density',(#4061),#7343);
#4137=REPRESENTATION('material name',(#4162),#7344);
#4138=REPRESENTATION('density',(#4062),#7344);
#4139=REPRESENTATION('material name',(#4163),#7345);
#4140=REPRESENTATION('density',(#4063),#7345);
#4141=REPRESENTATION('material name',(#4164),#7346);
#4142=REPRESENTATION('density',(#4064),#7346);
#4143=REPRESENTATION('material name',(#4165),#7347);
#4144=REPRESENTATION('density',(#4065),#7347);
#4145=REPRESENTATION('material name',(#4166),#7348);
#4146=REPRESENTATION('density',(#4066),#7348);
#4147=DESCRIPTIVE_REPRESENTATION_ITEM('Steel','Steel');
#4148=DESCRIPTIVE_REPRESENTATION_ITEM('Steel','Steel');
#4149=DESCRIPTIVE_REPRESENTATION_ITEM('Steel','Steel');
#4150=DESCRIPTIVE_REPRESENTATION_ITEM('Steel','Steel');
#4151=DESCRIPTIVE_REPRESENTATION_ITEM('Steel','Steel');
#4152=DESCRIPTIVE_REPRESENTATION_ITEM('Steel','Steel');
#4153=DESCRIPTIVE_REPRESENTATION_ITEM('Steel','Steel');
#4154=DESCRIPTIVE_REPRESENTATION_ITEM('Steel','Steel');
#4155=DESCRIPTIVE_REPRESENTATION_ITEM('Steel','Steel');
#4156=DESCRIPTIVE_REPRESENTATION_ITEM('Steel','Steel');
#4157=DESCRIPTIVE_REPRESENTATION_ITEM('Steel','Steel');
#4158=DESCRIPTIVE_REPRESENTATION_ITEM('Steel','Steel');
#4159=DESCRIPTIVE_REPRESENTATION_ITEM('Steel','Steel');
#4160=DESCRIPTIVE_REPRESENTATION_ITEM('Steel','Steel');
#4161=DESCRIPTIVE_REPRESENTATION_ITEM('Steel','Steel');
#4162=DESCRIPTIVE_REPRESENTATION_ITEM('Steel','Steel');
#4163=DESCRIPTIVE_REPRESENTATION_ITEM('Steel','Steel');
#4164=DESCRIPTIVE_REPRESENTATION_ITEM('Steel','Steel');
#4165=DESCRIPTIVE_REPRESENTATION_ITEM('Steel','Steel');
#4166=DESCRIPTIVE_REPRESENTATION_ITEM('Steel','Steel');
#4167=PROPERTY_DEFINITION('material property','material name',#7468);
#4168=PROPERTY_DEFINITION('material property','density of part',#7468);
#4169=PROPERTY_DEFINITION('material property','material name',#7469);
#4170=PROPERTY_DEFINITION('material property','density of part',#7469);
#4171=PROPERTY_DEFINITION('material property','material name',#7470);
#4172=PROPERTY_DEFINITION('material property','density of part',#7470);
#4173=PROPERTY_DEFINITION('material property','material name',#7471);
#4174=PROPERTY_DEFINITION('material property','density of part',#7471);
#4175=PROPERTY_DEFINITION('material property','material name',#7472);
#4176=PROPERTY_DEFINITION('material property','density of part',#7472);
#4177=PROPERTY_DEFINITION('material property','material name',#7473);
#4178=PROPERTY_DEFINITION('material property','density of part',#7473);
#4179=PROPERTY_DEFINITION('material property','material name',#7474);
#4180=PROPERTY_DEFINITION('material property','density of part',#7474);
#4181=PROPERTY_DEFINITION('material property','material name',#7475);
#4182=PROPERTY_DEFINITION('material property','density of part',#7475);
#4183=PROPERTY_DEFINITION('material property','material name',#7476);
#4184=PROPERTY_DEFINITION('material property','density of part',#7476);
#4185=PROPERTY_DEFINITION('material property','material name',#7477);
#4186=PROPERTY_DEFINITION('material property','density of part',#7477);
#4187=PROPERTY_DEFINITION('material property','material name',#7478);
#4188=PROPERTY_DEFINITION('material property','density of part',#7478);
#4189=PROPERTY_DEFINITION('material property','material name',#7479);
#4190=PROPERTY_DEFINITION('material property','density of part',#7479);
#4191=PROPERTY_DEFINITION('material property','material name',#7481);
#4192=PROPERTY_DEFINITION('material property','density of part',#7481);
#4193=PROPERTY_DEFINITION('material property','material name',#7482);
#4194=PROPERTY_DEFINITION('material property','density of part',#7482);
#4195=PROPERTY_DEFINITION('material property','material name',#7484);
#4196=PROPERTY_DEFINITION('material property','density of part',#7484);
#4197=PROPERTY_DEFINITION('material property','material name',#7485);
#4198=PROPERTY_DEFINITION('material property','density of part',#7485);
#4199=PROPERTY_DEFINITION('material property','material name',#7486);
#4200=PROPERTY_DEFINITION('material property','density of part',#7486);
#4201=PROPERTY_DEFINITION('material property','material name',#7487);
#4202=PROPERTY_DEFINITION('material property','density of part',#7487);
#4203=PROPERTY_DEFINITION('material property','material name',#7488);
#4204=PROPERTY_DEFINITION('material property','density of part',#7488);
#4205=PROPERTY_DEFINITION('material property','material name',#7489);
#4206=PROPERTY_DEFINITION('material property','density of part',#7489);
#4207=AXIS2_PLACEMENT_3D('',#5987,#4707,#4708);
#4208=AXIS2_PLACEMENT_3D('',#5988,#4709,#4710);
#4209=AXIS2_PLACEMENT_3D('',#5989,#4711,#4712);
#4210=AXIS2_PLACEMENT_3D('',#5990,#4713,#4714);
#4211=AXIS2_PLACEMENT_3D('',#5992,#4715,#4716);
#4212=AXIS2_PLACEMENT_3D('',#5995,#4718,#4719);
#4213=AXIS2_PLACEMENT_3D('',#5996,#4720,#4721);
#4214=AXIS2_PLACEMENT_3D('',#5998,#4722,#4723);
#4215=AXIS2_PLACEMENT_3D('',#6001,#4725,#4726);
#4216=AXIS2_PLACEMENT_3D('',#6002,#4727,#4728);
#4217=AXIS2_PLACEMENT_3D('',#6004,#4729,#4730);
#4218=AXIS2_PLACEMENT_3D('',#6007,#4732,#4733);
#4219=AXIS2_PLACEMENT_3D('',#6008,#4734,#4735);
#4220=AXIS2_PLACEMENT_3D('',#6010,#4736,#4737);
#4221=AXIS2_PLACEMENT_3D('',#6013,#4739,#4740);
#4222=AXIS2_PLACEMENT_3D('',#6014,#4741,#4742);
#4223=AXIS2_PLACEMENT_3D('',#6023,#4747,#4748);
#4224=AXIS2_PLACEMENT_3D('',#6029,#4752,#4753);
#4225=AXIS2_PLACEMENT_3D('',#6035,#4757,#4758);
#4226=AXIS2_PLACEMENT_3D('',#6038,#4761,#4762);
#4227=AXIS2_PLACEMENT_3D('',#6039,#4763,#4764);
#4228=AXIS2_PLACEMENT_3D('',#6040,#4765,#4766);
#4229=AXIS2_PLACEMENT_3D('',#6041,#4767,#4768);
#4230=AXIS2_PLACEMENT_3D('',#6046,#4770,#4771);
#4231=AXIS2_PLACEMENT_3D('',#6050,#4773,#4774);
#4232=AXIS2_PLACEMENT_3D('',#6053,#4776,#4777);
#4233=AXIS2_PLACEMENT_3D('',#6054,#4778,#4779);
#4234=AXIS2_PLACEMENT_3D('',#6055,#4780,#4781);
#4235=AXIS2_PLACEMENT_3D('',#6057,#4782,#4783);
#4236=AXIS2_PLACEMENT_3D('',#6058,#4784,#4785);
#4237=AXIS2_PLACEMENT_3D('',#6059,#4786,#4787);
#4238=AXIS2_PLACEMENT_3D('',#6064,#4789,#4790);
#4239=AXIS2_PLACEMENT_3D('',#6068,#4792,#4793);
#4240=AXIS2_PLACEMENT_3D('',#6071,#4795,#4796);
#4241=AXIS2_PLACEMENT_3D('',#6072,#4797,#4798);
#4242=AXIS2_PLACEMENT_3D('',#6073,#4799,#4800);
#4243=AXIS2_PLACEMENT_3D('',#6074,#4801,#4802);
#4244=AXIS2_PLACEMENT_3D('',#6075,#4803,#4804);
#4245=AXIS2_PLACEMENT_3D('',#6080,#4806,#4807);
#4246=AXIS2_PLACEMENT_3D('',#6084,#4809,#4810);
#4247=AXIS2_PLACEMENT_3D('',#6087,#4812,#4813);
#4248=AXIS2_PLACEMENT_3D('',#6088,#4814,#4815);
#4249=AXIS2_PLACEMENT_3D('',#6089,#4816,#4817);
#4250=AXIS2_PLACEMENT_3D('',#6090,#4818,#4819);
#4251=AXIS2_PLACEMENT_3D('',#6091,#4820,#4821);
#4252=AXIS2_PLACEMENT_3D('',#6093,#4822,#4823);
#4253=AXIS2_PLACEMENT_3D('',#6094,#4824,#4825);
#4254=AXIS2_PLACEMENT_3D('',#6095,#4826,#4827);
#4255=AXIS2_PLACEMENT_3D('',#6096,#4828,#4829);
#4256=AXIS2_PLACEMENT_3D('',#6097,#4830,#4831);
#4257=AXIS2_PLACEMENT_3D('',#6100,#4832,#4833);
#4258=AXIS2_PLACEMENT_3D('',#6102,#4834,#4835);
#4259=AXIS2_PLACEMENT_3D('',#6103,#4836,#4837);
#4260=AXIS2_PLACEMENT_3D('',#6104,#4838,#4839);
#4261=AXIS2_PLACEMENT_3D('',#6106,#4840,#4841);
#4262=AXIS2_PLACEMENT_3D('',#6110,#4843,#4844);
#4263=AXIS2_PLACEMENT_3D('',#6114,#4847,#4848);
#4264=AXIS2_PLACEMENT_3D('',#6115,#4849,#4850);
#4265=AXIS2_PLACEMENT_3D('',#6118,#4851,#4852);
#4266=AXIS2_PLACEMENT_3D('',#6119,#4853,#4854);
#4267=AXIS2_PLACEMENT_3D('',#6120,#4855,#4856);
#4268=AXIS2_PLACEMENT_3D('',#6122,#4857,#4858);
#4269=AXIS2_PLACEMENT_3D('',#6126,#4860,#4861);
#4270=AXIS2_PLACEMENT_3D('',#6130,#4864,#4865);
#4271=AXIS2_PLACEMENT_3D('',#6131,#4866,#4867);
#4272=AXIS2_PLACEMENT_3D('',#6134,#4868,#4869);
#4273=AXIS2_PLACEMENT_3D('',#6135,#4870,#4871);
#4274=AXIS2_PLACEMENT_3D('',#6136,#4872,#4873);
#4275=AXIS2_PLACEMENT_3D('',#6138,#4874,#4875);
#4276=AXIS2_PLACEMENT_3D('',#6142,#4877,#4878);
#4277=AXIS2_PLACEMENT_3D('',#6146,#4881,#4882);
#4278=AXIS2_PLACEMENT_3D('',#6147,#4883,#4884);
#4279=AXIS2_PLACEMENT_3D('',#6149,#4886,#4887);
#4280=AXIS2_PLACEMENT_3D('',#6150,#4888,#4889);
#4281=AXIS2_PLACEMENT_3D('',#6151,#4890,#4891);
#4282=AXIS2_PLACEMENT_3D('',#6152,#4892,#4893);
#4283=AXIS2_PLACEMENT_3D('',#6154,#4894,#4895);
#4284=AXIS2_PLACEMENT_3D('',#6156,#4897,#4898);
#4285=AXIS2_PLACEMENT_3D('',#6158,#4899,#4900);
#4286=AXIS2_PLACEMENT_3D('',#6159,#4901,#4902);
#4287=AXIS2_PLACEMENT_3D('',#6162,#4904,#4905);
#4288=AXIS2_PLACEMENT_3D('',#6163,#4906,#4907);
#4289=AXIS2_PLACEMENT_3D('',#6165,#4908,#4909);
#4290=AXIS2_PLACEMENT_3D('',#6168,#4911,#4912);
#4291=AXIS2_PLACEMENT_3D('',#6169,#4913,#4914);
#4292=AXIS2_PLACEMENT_3D('',#6170,#4915,#4916);
#4293=AXIS2_PLACEMENT_3D('',#6171,#4917,#4918);
#4294=AXIS2_PLACEMENT_3D('',#6172,#4919,#4920);
#4295=AXIS2_PLACEMENT_3D('',#6174,#4921,#4922);
#4296=AXIS2_PLACEMENT_3D('',#6177,#4924,#4925);
#4297=AXIS2_PLACEMENT_3D('',#6178,#4926,#4927);
#4298=AXIS2_PLACEMENT_3D('',#6179,#4928,#4929);
#4299=AXIS2_PLACEMENT_3D('',#6181,#4930,#4931);
#4300=AXIS2_PLACEMENT_3D('',#6184,#4933,#4934);
#4301=AXIS2_PLACEMENT_3D('',#6185,#4935,#4936);
#4302=AXIS2_PLACEMENT_3D('',#6186,#4937,#4938);
#4303=AXIS2_PLACEMENT_3D('',#6188,#4939,#4940);
#4304=AXIS2_PLACEMENT_3D('',#6191,#4942,#4943);
#4305=AXIS2_PLACEMENT_3D('',#6192,#4944,#4945);
#4306=AXIS2_PLACEMENT_3D('',#6193,#4946,#4947);
#4307=AXIS2_PLACEMENT_3D('',#6195,#4948,#4949);
#4308=AXIS2_PLACEMENT_3D('',#6198,#4951,#4952);
#4309=AXIS2_PLACEMENT_3D('',#6199,#4953,#4954);
#4310=AXIS2_PLACEMENT_3D('',#6200,#4955,#4956);
#4311=AXIS2_PLACEMENT_3D('',#6203,#4957,#4958);
#4312=AXIS2_PLACEMENT_3D('',#6207,#4960,#4961);
#4313=AXIS2_PLACEMENT_3D('',#6209,#4963,#4964);
#4314=AXIS2_PLACEMENT_3D('',#6219,#4970,#4971);
#4315=AXIS2_PLACEMENT_3D('',#6223,#4974,#4975);
#4316=AXIS2_PLACEMENT_3D('',#6229,#4979,#4980);
#4317=AXIS2_PLACEMENT_3D('',#6233,#4983,#4984);
#4318=AXIS2_PLACEMENT_3D('',#6236,#4987,#4988);
#4319=AXIS2_PLACEMENT_3D('',#6237,#4989,#4990);
#4320=AXIS2_PLACEMENT_3D('',#6238,#4991,#4992);
#4321=AXIS2_PLACEMENT_3D('',#6239,#4993,#4994);
#4322=AXIS2_PLACEMENT_3D('',#6243,#4996,#4997);
#4323=AXIS2_PLACEMENT_3D('',#6245,#4998,#4999);
#4324=AXIS2_PLACEMENT_3D('',#6246,#5000,#5001);
#4325=AXIS2_PLACEMENT_3D('',#6250,#5003,#5004);
#4326=AXIS2_PLACEMENT_3D('',#6252,#5006,#5007);
#4327=AXIS2_PLACEMENT_3D('',#6256,#5009,#5010);
#4328=AXIS2_PLACEMENT_3D('',#6258,#5011,#5012);
#4329=AXIS2_PLACEMENT_3D('',#6259,#5013,#5014);
#4330=AXIS2_PLACEMENT_3D('',#6263,#5016,#5017);
#4331=AXIS2_PLACEMENT_3D('',#6265,#5019,#5020);
#4332=AXIS2_PLACEMENT_3D('',#6275,#5026,#5027);
#4333=AXIS2_PLACEMENT_3D('',#6285,#5033,#5034);
#4334=AXIS2_PLACEMENT_3D('',#6287,#5035,#5036);
#4335=AXIS2_PLACEMENT_3D('',#6289,#5038,#5039);
#4336=AXIS2_PLACEMENT_3D('',#6291,#5040,#5041);
#4337=AXIS2_PLACEMENT_3D('',#6293,#5043,#5044);
#4338=AXIS2_PLACEMENT_3D('',#6296,#5045,#5046);
#4339=AXIS2_PLACEMENT_3D('',#6300,#5048,#5049);
#4340=AXIS2_PLACEMENT_3D('',#6302,#5051,#5052);
#4341=AXIS2_PLACEMENT_3D('',#6306,#5056,#5057);
#4342=AXIS2_PLACEMENT_3D('',#6308,#5059,#5060);
#4343=AXIS2_PLACEMENT_3D('',#6311,#5063,#5064);
#4344=AXIS2_PLACEMENT_3D('',#6312,#5065,#5066);
#4345=AXIS2_PLACEMENT_3D('',#6313,#5067,#5068);
#4346=AXIS2_PLACEMENT_3D('',#6314,#5069,#5070);
#4347=AXIS2_PLACEMENT_3D('',#6316,#5071,#5072);
#4348=AXIS2_PLACEMENT_3D('',#6319,#5074,#5075);
#4349=AXIS2_PLACEMENT_3D('',#6320,#5076,#5077);
#4350=AXIS2_PLACEMENT_3D('',#6321,#5078,#5079);
#4351=AXIS2_PLACEMENT_3D('',#6323,#5080,#5081);
#4352=AXIS2_PLACEMENT_3D('',#6326,#5083,#5084);
#4353=AXIS2_PLACEMENT_3D('',#6327,#5085,#5086);
#4354=AXIS2_PLACEMENT_3D('',#6328,#5087,#5088);
#4355=AXIS2_PLACEMENT_3D('',#6330,#5089,#5090);
#4356=AXIS2_PLACEMENT_3D('',#6333,#5092,#5093);
#4357=AXIS2_PLACEMENT_3D('',#6334,#5094,#5095);
#4358=AXIS2_PLACEMENT_3D('',#6335,#5096,#5097);
#4359=AXIS2_PLACEMENT_3D('',#6337,#5098,#5099);
#4360=AXIS2_PLACEMENT_3D('',#6340,#5101,#5102);
#4361=AXIS2_PLACEMENT_3D('',#6341,#5103,#5104);
#4362=AXIS2_PLACEMENT_3D('',#6342,#5105,#5106);
#4363=AXIS2_PLACEMENT_3D('',#6345,#5107,#5108);
#4364=AXIS2_PLACEMENT_3D('',#6349,#5110,#5111);
#4365=AXIS2_PLACEMENT_3D('',#6351,#5113,#5114);
#4366=AXIS2_PLACEMENT_3D('',#6361,#5120,#5121);
#4367=AXIS2_PLACEMENT_3D('',#6365,#5124,#5125);
#4368=AXIS2_PLACEMENT_3D('',#6371,#5129,#5130);
#4369=AXIS2_PLACEMENT_3D('',#6375,#5133,#5134);
#4370=AXIS2_PLACEMENT_3D('',#6378,#5137,#5138);
#4371=AXIS2_PLACEMENT_3D('',#6379,#5139,#5140);
#4372=AXIS2_PLACEMENT_3D('',#6380,#5141,#5142);
#4373=AXIS2_PLACEMENT_3D('',#6381,#5143,#5144);
#4374=AXIS2_PLACEMENT_3D('',#6385,#5146,#5147);
#4375=AXIS2_PLACEMENT_3D('',#6387,#5148,#5149);
#4376=AXIS2_PLACEMENT_3D('',#6388,#5150,#5151);
#4377=AXIS2_PLACEMENT_3D('',#6392,#5153,#5154);
#4378=AXIS2_PLACEMENT_3D('',#6394,#5156,#5157);
#4379=AXIS2_PLACEMENT_3D('',#6398,#5159,#5160);
#4380=AXIS2_PLACEMENT_3D('',#6400,#5161,#5162);
#4381=AXIS2_PLACEMENT_3D('',#6401,#5163,#5164);
#4382=AXIS2_PLACEMENT_3D('',#6405,#5166,#5167);
#4383=AXIS2_PLACEMENT_3D('',#6407,#5169,#5170);
#4384=AXIS2_PLACEMENT_3D('',#6417,#5176,#5177);
#4385=AXIS2_PLACEMENT_3D('',#6427,#5183,#5184);
#4386=AXIS2_PLACEMENT_3D('',#6429,#5185,#5186);
#4387=AXIS2_PLACEMENT_3D('',#6431,#5188,#5189);
#4388=AXIS2_PLACEMENT_3D('',#6433,#5190,#5191);
#4389=AXIS2_PLACEMENT_3D('',#6435,#5193,#5194);
#4390=AXIS2_PLACEMENT_3D('',#6438,#5195,#5196);
#4391=AXIS2_PLACEMENT_3D('',#6442,#5198,#5199);
#4392=AXIS2_PLACEMENT_3D('',#6444,#5201,#5202);
#4393=AXIS2_PLACEMENT_3D('',#6448,#5206,#5207);
#4394=AXIS2_PLACEMENT_3D('',#6450,#5209,#5210);
#4395=AXIS2_PLACEMENT_3D('',#6453,#5213,#5214);
#4396=AXIS2_PLACEMENT_3D('',#6454,#5215,#5216);
#4397=AXIS2_PLACEMENT_3D('',#6455,#5217,#5218);
#4398=AXIS2_PLACEMENT_3D('',#6456,#5219,#5220);
#4399=AXIS2_PLACEMENT_3D('',#6458,#5221,#5222);
#4400=AXIS2_PLACEMENT_3D('',#6461,#5224,#5225);
#4401=AXIS2_PLACEMENT_3D('',#6462,#5226,#5227);
#4402=AXIS2_PLACEMENT_3D('',#6464,#5228,#5229);
#4403=AXIS2_PLACEMENT_3D('',#6467,#5231,#5232);
#4404=AXIS2_PLACEMENT_3D('',#6468,#5233,#5234);
#4405=AXIS2_PLACEMENT_3D('',#6469,#5235,#5236);
#4406=AXIS2_PLACEMENT_3D('',#6470,#5237,#5238);
#4407=AXIS2_PLACEMENT_3D('',#6471,#5239,#5240);
#4408=AXIS2_PLACEMENT_3D('',#6473,#5241,#5242);
#4409=AXIS2_PLACEMENT_3D('',#6476,#5244,#5245);
#4410=AXIS2_PLACEMENT_3D('',#6477,#5246,#5247);
#4411=AXIS2_PLACEMENT_3D('',#6479,#5248,#5249);
#4412=AXIS2_PLACEMENT_3D('',#6482,#5251,#5252);
#4413=AXIS2_PLACEMENT_3D('',#6483,#5253,#5254);
#4414=AXIS2_PLACEMENT_3D('',#6484,#5255,#5256);
#4415=AXIS2_PLACEMENT_3D('',#6485,#5257,#5258);
#4416=AXIS2_PLACEMENT_3D('',#6486,#5259,#5260);
#4417=AXIS2_PLACEMENT_3D('',#6488,#5261,#5262);
#4418=AXIS2_PLACEMENT_3D('',#6491,#5264,#5265);
#4419=AXIS2_PLACEMENT_3D('',#6492,#5266,#5267);
#4420=AXIS2_PLACEMENT_3D('',#6494,#5268,#5269);
#4421=AXIS2_PLACEMENT_3D('',#6497,#5271,#5272);
#4422=AXIS2_PLACEMENT_3D('',#6498,#5273,#5274);
#4423=AXIS2_PLACEMENT_3D('',#6499,#5275,#5276);
#4424=AXIS2_PLACEMENT_3D('',#6500,#5277,#5278);
#4425=AXIS2_PLACEMENT_3D('',#6501,#5279,#5280);
#4426=AXIS2_PLACEMENT_3D('',#6503,#5281,#5282);
#4427=AXIS2_PLACEMENT_3D('',#6506,#5284,#5285);
#4428=AXIS2_PLACEMENT_3D('',#6507,#5286,#5287);
#4429=AXIS2_PLACEMENT_3D('',#6509,#5288,#5289);
#4430=AXIS2_PLACEMENT_3D('',#6512,#5291,#5292);
#4431=AXIS2_PLACEMENT_3D('',#6513,#5293,#5294);
#4432=AXIS2_PLACEMENT_3D('',#6515,#5295,#5296);
#4433=AXIS2_PLACEMENT_3D('',#6518,#5298,#5299);
#4434=AXIS2_PLACEMENT_3D('',#6519,#5300,#5301);
#4435=AXIS2_PLACEMENT_3D('',#6521,#5302,#5303);
#4436=AXIS2_PLACEMENT_3D('',#6524,#5305,#5306);
#4437=AXIS2_PLACEMENT_3D('',#6525,#5307,#5308);
#4438=AXIS2_PLACEMENT_3D('',#6527,#5309,#5310);
#4439=AXIS2_PLACEMENT_3D('',#6528,#5311,#5312);
#4440=AXIS2_PLACEMENT_3D('',#6530,#5313,#5314);
#4441=AXIS2_PLACEMENT_3D('',#6532,#5316,#5317);
#4442=AXIS2_PLACEMENT_3D('',#6534,#5318,#5319);
#4443=AXIS2_PLACEMENT_3D('',#6537,#5321,#5322);
#4444=AXIS2_PLACEMENT_3D('',#6538,#5323,#5324);
#4445=AXIS2_PLACEMENT_3D('',#6539,#5325,#5326);
#4446=AXIS2_PLACEMENT_3D('',#6540,#5327,#5328);
#4447=AXIS2_PLACEMENT_3D('',#6541,#5329,#5330);
#4448=AXIS2_PLACEMENT_3D('',#6545,#5332,#5333);
#4449=AXIS2_PLACEMENT_3D('',#6546,#5334,#5335);
#4450=AXIS2_PLACEMENT_3D('',#6548,#5336,#5337);
#4451=AXIS2_PLACEMENT_3D('',#6585,#5339,#5340);
#4452=AXIS2_PLACEMENT_3D('',#6630,#5342,#5343);
#4453=AXIS2_PLACEMENT_3D('',#6631,#5344,#5345);
#4454=AXIS2_PLACEMENT_3D('',#6634,#5346,#5347);
#4455=AXIS2_PLACEMENT_3D('',#6635,#5348,#5349);
#4456=AXIS2_PLACEMENT_3D('',#6636,#5350,#5351);
#4457=AXIS2_PLACEMENT_3D('',#6638,#5352,#5353);
#4458=AXIS2_PLACEMENT_3D('',#6642,#5355,#5356);
#4459=AXIS2_PLACEMENT_3D('',#6646,#5359,#5360);
#4460=AXIS2_PLACEMENT_3D('',#6647,#5361,#5362);
#4461=AXIS2_PLACEMENT_3D('',#6650,#5363,#5364);
#4462=AXIS2_PLACEMENT_3D('',#6651,#5365,#5366);
#4463=AXIS2_PLACEMENT_3D('',#6652,#5367,#5368);
#4464=AXIS2_PLACEMENT_3D('',#6654,#5369,#5370);
#4465=AXIS2_PLACEMENT_3D('',#6658,#5372,#5373);
#4466=AXIS2_PLACEMENT_3D('',#6662,#5376,#5377);
#4467=AXIS2_PLACEMENT_3D('',#6663,#5378,#5379);
#4468=AXIS2_PLACEMENT_3D('',#6666,#5380,#5381);
#4469=AXIS2_PLACEMENT_3D('',#6667,#5382,#5383);
#4470=AXIS2_PLACEMENT_3D('',#6668,#5384,#5385);
#4471=AXIS2_PLACEMENT_3D('',#6670,#5386,#5387);
#4472=AXIS2_PLACEMENT_3D('',#6674,#5389,#5390);
#4473=AXIS2_PLACEMENT_3D('',#6678,#5393,#5394);
#4474=AXIS2_PLACEMENT_3D('',#6679,#5395,#5396);
#4475=AXIS2_PLACEMENT_3D('',#6680,#5397,#5398);
#4476=AXIS2_PLACEMENT_3D('',#6681,#5399,#5400);
#4477=AXIS2_PLACEMENT_3D('',#6683,#5401,#5402);
#4478=AXIS2_PLACEMENT_3D('',#6687,#5404,#5405);
#4479=AXIS2_PLACEMENT_3D('',#6690,#5407,#5408);
#4480=AXIS2_PLACEMENT_3D('',#6691,#5409,#5410);
#4481=AXIS2_PLACEMENT_3D('',#6697,#5414,#5415);
#4482=AXIS2_PLACEMENT_3D('',#6703,#5419,#5420);
#4483=AXIS2_PLACEMENT_3D('',#6705,#5421,#5422);
#4484=AXIS2_PLACEMENT_3D('',#6706,#5423,#5424);
#4485=AXIS2_PLACEMENT_3D('',#6707,#5425,#5426);
#4486=AXIS2_PLACEMENT_3D('',#6709,#5427,#5428);
#4487=AXIS2_PLACEMENT_3D('',#6710,#5429,#5430);
#4488=AXIS2_PLACEMENT_3D('',#6711,#5431,#5432);
#4489=AXIS2_PLACEMENT_3D('',#6714,#5434,#5435);
#4490=AXIS2_PLACEMENT_3D('',#6715,#5436,#5437);
#4491=AXIS2_PLACEMENT_3D('',#6718,#5439,#5440);
#4492=AXIS2_PLACEMENT_3D('',#6719,#5441,#5442);
#4493=AXIS2_PLACEMENT_3D('',#6720,#5443,#5444);
#4494=AXIS2_PLACEMENT_3D('',#6721,#5445,#5446);
#4495=AXIS2_PLACEMENT_3D('',#6723,#5447,#5448);
#4496=AXIS2_PLACEMENT_3D('',#6724,#5449,#5450);
#4497=AXIS2_PLACEMENT_3D('',#6726,#5451,#5452);
#4498=AXIS2_PLACEMENT_3D('',#6728,#5454,#5455);
#4499=AXIS2_PLACEMENT_3D('',#6730,#5456,#5457);
#4500=AXIS2_PLACEMENT_3D('',#6732,#5459,#5460);
#4501=AXIS2_PLACEMENT_3D('',#6734,#5461,#5462);
#4502=AXIS2_PLACEMENT_3D('',#6736,#5464,#5465);
#4503=AXIS2_PLACEMENT_3D('',#6738,#5466,#5467);
#4504=AXIS2_PLACEMENT_3D('',#6739,#5468,#5469);
#4505=AXIS2_PLACEMENT_3D('',#6741,#5470,#5471);
#4506=AXIS2_PLACEMENT_3D('',#6743,#5473,#5474);
#4507=AXIS2_PLACEMENT_3D('',#6745,#5475,#5476);
#4508=AXIS2_PLACEMENT_3D('',#6747,#5478,#5479);
#4509=AXIS2_PLACEMENT_3D('',#6749,#5480,#5481);
#4510=AXIS2_PLACEMENT_3D('',#6751,#5483,#5484);
#4511=AXIS2_PLACEMENT_3D('',#6752,#5485,#5486);
#4512=AXIS2_PLACEMENT_3D('',#6761,#5491,#5492);
#4513=AXIS2_PLACEMENT_3D('',#6767,#5496,#5497);
#4514=AXIS2_PLACEMENT_3D('',#6773,#5501,#5502);
#4515=AXIS2_PLACEMENT_3D('',#6779,#5506,#5507);
#4516=AXIS2_PLACEMENT_3D('',#6785,#5511,#5512);
#4517=AXIS2_PLACEMENT_3D('',#6788,#5515,#5516);
#4518=AXIS2_PLACEMENT_3D('',#6789,#5517,#5518);
#4519=AXIS2_PLACEMENT_3D('',#6790,#5519,#5520);
#4520=AXIS2_PLACEMENT_3D('',#6791,#5521,#5522);
#4521=AXIS2_PLACEMENT_3D('',#6792,#5523,#5524);
#4522=AXIS2_PLACEMENT_3D('',#6795,#5525,#5526);
#4523=AXIS2_PLACEMENT_3D('',#6801,#5530,#5531);
#4524=AXIS2_PLACEMENT_3D('',#6807,#5535,#5536);
#4525=AXIS2_PLACEMENT_3D('',#6809,#5537,#5538);
#4526=AXIS2_PLACEMENT_3D('',#6813,#5541,#5542);
#4527=AXIS2_PLACEMENT_3D('',#6816,#5545,#5546);
#4528=AXIS2_PLACEMENT_3D('',#6817,#5547,#5548);
#4529=AXIS2_PLACEMENT_3D('',#6819,#5549,#5550);
#4530=AXIS2_PLACEMENT_3D('',#6821,#5551,#5552);
#4531=AXIS2_PLACEMENT_3D('',#6822,#5553,#5554);
#4532=AXIS2_PLACEMENT_3D('',#6824,#5555,#5556);
#4533=AXIS2_PLACEMENT_3D('',#6826,#5558,#5559);
#4534=AXIS2_PLACEMENT_3D('',#6828,#5560,#5561);
#4535=AXIS2_PLACEMENT_3D('',#6829,#5562,#5563);
#4536=AXIS2_PLACEMENT_3D('',#6831,#5564,#5565);
#4537=AXIS2_PLACEMENT_3D('',#6833,#5567,#5568);
#4538=AXIS2_PLACEMENT_3D('',#6835,#5569,#5570);
#4539=AXIS2_PLACEMENT_3D('',#6836,#5571,#5572);
#4540=AXIS2_PLACEMENT_3D('',#6838,#5573,#5574);
#4541=AXIS2_PLACEMENT_3D('',#6840,#5576,#5577);
#4542=AXIS2_PLACEMENT_3D('',#6842,#5578,#5579);
#4543=AXIS2_PLACEMENT_3D('',#6843,#5580,#5581);
#4544=AXIS2_PLACEMENT_3D('',#6845,#5582,#5583);
#4545=AXIS2_PLACEMENT_3D('',#6847,#5585,#5586);
#4546=AXIS2_PLACEMENT_3D('',#6849,#5587,#5588);
#4547=AXIS2_PLACEMENT_3D('',#6850,#5589,#5590);
#4548=AXIS2_PLACEMENT_3D('',#6852,#5591,#5592);
#4549=AXIS2_PLACEMENT_3D('',#6854,#5594,#5595);
#4550=AXIS2_PLACEMENT_3D('',#6856,#5596,#5597);
#4551=AXIS2_PLACEMENT_3D('',#6857,#5598,#5599);
#4552=AXIS2_PLACEMENT_3D('',#6859,#5601,#5602);
#4553=AXIS2_PLACEMENT_3D('',#6860,#5603,#5604);
#4554=AXIS2_PLACEMENT_3D('',#6863,#5605,#5606);
#4555=AXIS2_PLACEMENT_3D('',#6867,#5608,#5609);
#4556=AXIS2_PLACEMENT_3D('',#6869,#5611,#5612);
#4557=AXIS2_PLACEMENT_3D('',#6875,#5616,#5617);
#4558=AXIS2_PLACEMENT_3D('',#6877,#5618,#5619);
#4559=AXIS2_PLACEMENT_3D('',#6879,#5620,#5621);
#4560=AXIS2_PLACEMENT_3D('',#6881,#5623,#5624);
#4561=AXIS2_PLACEMENT_3D('',#6884,#5627,#5628);
#4562=AXIS2_PLACEMENT_3D('',#6886,#5629,#5630);
#4563=AXIS2_PLACEMENT_3D('',#6888,#5631,#5632);
#4564=AXIS2_PLACEMENT_3D('',#6889,#5633,#5634);
#4565=AXIS2_PLACEMENT_3D('',#6891,#5635,#5636);
#4566=AXIS2_PLACEMENT_3D('',#6893,#5638,#5639);
#4567=AXIS2_PLACEMENT_3D('',#6895,#5640,#5641);
#4568=AXIS2_PLACEMENT_3D('',#6896,#5642,#5643);
#4569=AXIS2_PLACEMENT_3D('',#6898,#5645,#5646);
#4570=AXIS2_PLACEMENT_3D('',#6899,#5647,#5648);
#4571=AXIS2_PLACEMENT_3D('',#6900,#5649,#5650);
#4572=AXIS2_PLACEMENT_3D('',#6901,#5651,#5652);
#4573=AXIS2_PLACEMENT_3D('',#6902,#5653,#5654);
#4574=AXIS2_PLACEMENT_3D('',#6906,#5656,#5657);
#4575=AXIS2_PLACEMENT_3D('',#6907,#5658,#5659);
#4576=AXIS2_PLACEMENT_3D('',#6917,#5660,#5661);
#4577=AXIS2_PLACEMENT_3D('',#6979,#5663,#5664);
#4578=AXIS2_PLACEMENT_3D('',#6981,#5666,#5667);
#4579=AXIS2_PLACEMENT_3D('',#6983,#5668,#5669);
#4580=AXIS2_PLACEMENT_3D('',#6987,#5672,#5673);
#4581=AXIS2_PLACEMENT_3D('',#6988,#5674,#5675);
#4582=AXIS2_PLACEMENT_3D('',#6990,#5676,#5677);
#4583=AXIS2_PLACEMENT_3D('',#6994,#5680,#5681);
#4584=AXIS2_PLACEMENT_3D('',#6995,#5682,#5683);
#4585=AXIS2_PLACEMENT_3D('',#6996,#5684,#5685);
#4586=AXIS2_PLACEMENT_3D('',#6997,#5686,#5687);
#4587=AXIS2_PLACEMENT_3D('',#6998,#5688,#5689);
#4588=AXIS2_PLACEMENT_3D('',#7002,#5691,#5692);
#4589=AXIS2_PLACEMENT_3D('',#7003,#5693,#5694);
#4590=AXIS2_PLACEMENT_3D('',#7013,#5695,#5696);
#4591=AXIS2_PLACEMENT_3D('',#7075,#5698,#5699);
#4592=AXIS2_PLACEMENT_3D('',#7077,#5701,#5702);
#4593=AXIS2_PLACEMENT_3D('',#7079,#5703,#5704);
#4594=AXIS2_PLACEMENT_3D('',#7083,#5707,#5708);
#4595=AXIS2_PLACEMENT_3D('',#7084,#5709,#5710);
#4596=AXIS2_PLACEMENT_3D('',#7086,#5711,#5712);
#4597=AXIS2_PLACEMENT_3D('',#7090,#5715,#5716);
#4598=AXIS2_PLACEMENT_3D('',#7091,#5717,#5718);
#4599=AXIS2_PLACEMENT_3D('',#7092,#5719,#5720);
#4600=AXIS2_PLACEMENT_3D('',#7093,#5721,#5722);
#4601=AXIS2_PLACEMENT_3D('',#7094,#5723,#5724);
#4602=AXIS2_PLACEMENT_3D('',#7096,#5725,#5726);
#4603=AXIS2_PLACEMENT_3D('',#7099,#5728,#5729);
#4604=AXIS2_PLACEMENT_3D('',#7100,#5730,#5731);
#4605=AXIS2_PLACEMENT_3D('',#7102,#5732,#5733);
#4606=AXIS2_PLACEMENT_3D('',#7103,#5734,#5735);
#4607=AXIS2_PLACEMENT_3D('',#7106,#5737,#5738);
#4608=AXIS2_PLACEMENT_3D('',#7107,#5739,#5740);
#4609=AXIS2_PLACEMENT_3D('',#7109,#5741,#5742);
#4610=AXIS2_PLACEMENT_3D('',#7112,#5744,#5745);
#4611=AXIS2_PLACEMENT_3D('',#7113,#5746,#5747);
#4612=AXIS2_PLACEMENT_3D('',#7114,#5748,#5749);
#4613=AXIS2_PLACEMENT_3D('',#7115,#5750,#5751);
#4614=AXIS2_PLACEMENT_3D('',#7116,#5752,#5753);
#4615=AXIS2_PLACEMENT_3D('',#7118,#5754,#5755);
#4616=AXIS2_PLACEMENT_3D('',#7121,#5757,#5758);
#4617=AXIS2_PLACEMENT_3D('',#7122,#5759,#5760);
#4618=AXIS2_PLACEMENT_3D('',#7123,#5761,#5762);
#4619=AXIS2_PLACEMENT_3D('',#7125,#5763,#5764);
#4620=AXIS2_PLACEMENT_3D('',#7128,#5766,#5767);
#4621=AXIS2_PLACEMENT_3D('',#7129,#5768,#5769);
#4622=AXIS2_PLACEMENT_3D('',#7131,#5770,#5771);
#4623=AXIS2_PLACEMENT_3D('',#7133,#5773,#5774);
#4624=AXIS2_PLACEMENT_3D('',#7134,#5775,#5776);
#4625=AXIS2_PLACEMENT_3D('',#7136,#5777,#5778);
#4626=AXIS2_PLACEMENT_3D('',#7138,#5780,#5781);
#4627=AXIS2_PLACEMENT_3D('',#7139,#5782,#5783);
#4628=AXIS2_PLACEMENT_3D('',#7140,#5784,#5785);
#4629=AXIS2_PLACEMENT_3D('',#7149,#5790,#5791);
#4630=AXIS2_PLACEMENT_3D('',#7155,#5795,#5796);
#4631=AXIS2_PLACEMENT_3D('',#7161,#5800,#5801);
#4632=AXIS2_PLACEMENT_3D('',#7167,#5805,#5806);
#4633=AXIS2_PLACEMENT_3D('',#7173,#5810,#5811);
#4634=AXIS2_PLACEMENT_3D('',#7176,#5814,#5815);
#4635=AXIS2_PLACEMENT_3D('',#7177,#5816,#5817);
#4636=AXIS2_PLACEMENT_3D('',#7179,#5818,#5819);
#4637=AXIS2_PLACEMENT_3D('',#7180,#5820,#5821);
#4638=AXIS2_PLACEMENT_3D('',#7182,#5822,#5823);
#4639=AXIS2_PLACEMENT_3D('',#7184,#5825,#5826);
#4640=AXIS2_PLACEMENT_3D('',#7186,#5827,#5828);
#4641=AXIS2_PLACEMENT_3D('',#7188,#5830,#5831);
#4642=AXIS2_PLACEMENT_3D('',#7190,#5832,#5833);
#4643=AXIS2_PLACEMENT_3D('',#7192,#5835,#5836);
#4644=AXIS2_PLACEMENT_3D('',#7193,#5837,#5838);
#4645=AXIS2_PLACEMENT_3D('',#7194,#5839,#5840);
#4646=AXIS2_PLACEMENT_3D('',#7196,#5841,#5842);
#4647=AXIS2_PLACEMENT_3D('',#7197,#5843,#5844);
#4648=AXIS2_PLACEMENT_3D('',#7199,#5845,#5846);
#4649=AXIS2_PLACEMENT_3D('',#7201,#5848,#5849);
#4650=AXIS2_PLACEMENT_3D('',#7203,#5850,#5851);
#4651=AXIS2_PLACEMENT_3D('',#7205,#5853,#5854);
#4652=AXIS2_PLACEMENT_3D('',#7207,#5855,#5856);
#4653=AXIS2_PLACEMENT_3D('',#7209,#5858,#5859);
#4654=AXIS2_PLACEMENT_3D('',#7211,#5860,#5861);
#4655=AXIS2_PLACEMENT_3D('',#7212,#5862,#5863);
#4656=AXIS2_PLACEMENT_3D('',#7214,#5864,#5865);
#4657=AXIS2_PLACEMENT_3D('',#7216,#5867,#5868);
#4658=AXIS2_PLACEMENT_3D('',#7218,#5869,#5870);
#4659=AXIS2_PLACEMENT_3D('',#7220,#5872,#5873);
#4660=AXIS2_PLACEMENT_3D('',#7222,#5874,#5875);
#4661=AXIS2_PLACEMENT_3D('',#7224,#5877,#5878);
#4662=AXIS2_PLACEMENT_3D('',#7225,#5879,#5880);
#4663=AXIS2_PLACEMENT_3D('',#7234,#5885,#5886);
#4664=AXIS2_PLACEMENT_3D('',#7240,#5890,#5891);
#4665=AXIS2_PLACEMENT_3D('',#7246,#5895,#5896);
#4666=AXIS2_PLACEMENT_3D('',#7252,#5900,#5901);
#4667=AXIS2_PLACEMENT_3D('',#7258,#5905,#5906);
#4668=AXIS2_PLACEMENT_3D('',#7261,#5909,#5910);
#4669=AXIS2_PLACEMENT_3D('',#7262,#5911,#5912);
#4670=AXIS2_PLACEMENT_3D('',#7263,#5913,#5914);
#4671=AXIS2_PLACEMENT_3D('',#7264,#5915,#5916);
#4672=AXIS2_PLACEMENT_3D('',#7265,#5917,#5918);
#4673=AXIS2_PLACEMENT_3D('',#7266,#5919,#5920);
#4674=AXIS2_PLACEMENT_3D('',#7267,#5921,#5922);
#4675=AXIS2_PLACEMENT_3D('',#7268,#5923,#5924);
#4676=AXIS2_PLACEMENT_3D('',#7269,#5925,#5926);
#4677=AXIS2_PLACEMENT_3D('',#7270,#5927,#5928);
#4678=AXIS2_PLACEMENT_3D('',#7271,#5929,#5930);
#4679=AXIS2_PLACEMENT_3D('',#7272,#5931,#5932);
#4680=AXIS2_PLACEMENT_3D('',#7273,#5933,#5934);
#4681=AXIS2_PLACEMENT_3D('',#7274,#5935,#5936);
#4682=AXIS2_PLACEMENT_3D('',#7275,#5937,#5938);
#4683=AXIS2_PLACEMENT_3D('',#7276,#5939,#5940);
#4684=AXIS2_PLACEMENT_3D('',#7277,#5941,#5942);
#4685=AXIS2_PLACEMENT_3D('',#7278,#5943,#5944);
#4686=AXIS2_PLACEMENT_3D('',#7279,#5945,#5946);
#4687=AXIS2_PLACEMENT_3D('',#7280,#5947,#5948);
#4688=AXIS2_PLACEMENT_3D('',#7281,#5949,#5950);
#4689=AXIS2_PLACEMENT_3D('',#7282,#5951,#5952);
#4690=AXIS2_PLACEMENT_3D('',#7283,#5953,#5954);
#4691=AXIS2_PLACEMENT_3D('',#7284,#5955,#5956);
#4692=AXIS2_PLACEMENT_3D('',#7285,#5957,#5958);
#4693=AXIS2_PLACEMENT_3D('',#7286,#5959,#5960);
#4694=AXIS2_PLACEMENT_3D('',#7287,#5961,#5962);
#4695=AXIS2_PLACEMENT_3D('',#7288,#5963,#5964);
#4696=AXIS2_PLACEMENT_3D('',#7289,#5965,#5966);
#4697=AXIS2_PLACEMENT_3D('',#7290,#5967,#5968);
#4698=AXIS2_PLACEMENT_3D('',#7291,#5969,#5970);
#4699=AXIS2_PLACEMENT_3D('',#7292,#5971,#5972);
#4700=AXIS2_PLACEMENT_3D('',#7293,#5973,#5974);
#4701=AXIS2_PLACEMENT_3D('',#7294,#5975,#5976);
#4702=AXIS2_PLACEMENT_3D('',#7295,#5977,#5978);
#4703=AXIS2_PLACEMENT_3D('',#7296,#5979,#5980);
#4704=AXIS2_PLACEMENT_3D('',#7297,#5981,#5982);
#4705=AXIS2_PLACEMENT_3D('',#7298,#5983,#5984);
#4706=AXIS2_PLACEMENT_3D('',#7299,#5985,#5986);
#4707=DIRECTION('axis',(0.,0.,1.));
#4708=DIRECTION('refdir',(1.,0.,0.));
#4709=DIRECTION('axis',(0.,0.,1.));
#4710=DIRECTION('refdir',(1.,0.,0.));
#4711=DIRECTION('axis',(0.,0.,1.));
#4712=DIRECTION('refdir',(1.,0.,0.));
#4713=DIRECTION('center_axis',(0.,0.,1.));
#4714=DIRECTION('ref_axis',(1.,0.,0.));
#4715=DIRECTION('center_axis',(0.,0.,1.));
#4716=DIRECTION('ref_axis',(1.,0.,0.));
#4717=DIRECTION('',(0.,0.,1.));
#4718=DIRECTION('center_axis',(0.,0.,-1.));
#4719=DIRECTION('ref_axis',(1.,0.,0.));
#4720=DIRECTION('center_axis',(0.,0.,1.));
#4721=DIRECTION('ref_axis',(1.,0.,0.));
#4722=DIRECTION('center_axis',(0.,0.,1.));
#4723=DIRECTION('ref_axis',(1.,0.,0.));
#4724=DIRECTION('',(0.,0.,1.));
#4725=DIRECTION('center_axis',(0.,0.,-1.));
#4726=DIRECTION('ref_axis',(1.,0.,0.));
#4727=DIRECTION('center_axis',(0.,0.,1.));
#4728=DIRECTION('ref_axis',(1.,0.,0.));
#4729=DIRECTION('center_axis',(0.,0.,1.));
#4730=DIRECTION('ref_axis',(1.,0.,0.));
#4731=DIRECTION('',(0.,0.,1.));
#4732=DIRECTION('center_axis',(0.,0.,-1.));
#4733=DIRECTION('ref_axis',(1.,0.,0.));
#4734=DIRECTION('center_axis',(0.,0.,1.));
#4735=DIRECTION('ref_axis',(1.,0.,0.));
#4736=DIRECTION('center_axis',(0.,0.,1.));
#4737=DIRECTION('ref_axis',(1.,0.,0.));
#4738=DIRECTION('',(0.,0.,1.));
#4739=DIRECTION('center_axis',(0.,0.,-1.));
#4740=DIRECTION('ref_axis',(1.,0.,0.));
#4741=DIRECTION('center_axis',(0.,1.,0.));
#4742=DIRECTION('ref_axis',(-1.,0.,0.));
#4743=DIRECTION('',(-1.,0.,0.));
#4744=DIRECTION('',(0.,0.,1.));
#4745=DIRECTION('',(-1.,0.,0.));
#4746=DIRECTION('',(0.,0.,1.));
#4747=DIRECTION('center_axis',(1.,0.,0.));
#4748=DIRECTION('ref_axis',(0.,1.,0.));
#4749=DIRECTION('',(0.,1.,0.));
#4750=DIRECTION('',(0.,1.,0.));
#4751=DIRECTION('',(0.,0.,1.));
#4752=DIRECTION('center_axis',(0.,-1.,0.));
#4753=DIRECTION('ref_axis',(1.,0.,0.));
#4754=DIRECTION('',(1.,0.,0.));
#4755=DIRECTION('',(1.,0.,0.));
#4756=DIRECTION('',(0.,0.,1.));
#4757=DIRECTION('center_axis',(-1.,0.,0.));
#4758=DIRECTION('ref_axis',(0.,-1.,0.));
#4759=DIRECTION('',(0.,-1.,0.));
#4760=DIRECTION('',(0.,-1.,0.));
#4761=DIRECTION('center_axis',(0.,0.,1.));
#4762=DIRECTION('ref_axis',(1.,0.,0.));
#4763=DIRECTION('center_axis',(0.,0.,1.));
#4764=DIRECTION('ref_axis',(1.,0.,0.));
#4765=DIRECTION('axis',(0.,0.,1.));
#4766=DIRECTION('refdir',(1.,0.,0.));
#4767=DIRECTION('center_axis',(1.,0.,0.));
#4768=DIRECTION('ref_axis',(0.,0.,-1.));
#4769=DIRECTION('',(1.,0.,0.));
#4770=DIRECTION('center_axis',(1.,0.,0.));
#4771=DIRECTION('ref_axis',(0.,0.,-1.));
#4772=DIRECTION('',(-1.,0.,0.));
#4773=DIRECTION('center_axis',(1.,0.,0.));
#4774=DIRECTION('ref_axis',(0.,0.,-1.));
#4775=DIRECTION('',(1.,0.,0.));
#4776=DIRECTION('center_axis',(-1.,0.,0.));
#4777=DIRECTION('ref_axis',(0.,0.,-1.));
#4778=DIRECTION('center_axis',(1.,0.,0.));
#4779=DIRECTION('ref_axis',(0.,0.,-1.));
#4780=DIRECTION('center_axis',(1.,0.,0.));
#4781=DIRECTION('ref_axis',(0.,0.,-1.));
#4782=DIRECTION('center_axis',(-1.,0.,0.));
#4783=DIRECTION('ref_axis',(0.,0.,-1.));
#4784=DIRECTION('center_axis',(-1.,0.,0.));
#4785=DIRECTION('ref_axis',(0.,0.,-1.));
#4786=DIRECTION('center_axis',(1.,0.,0.));
#4787=DIRECTION('ref_axis',(0.,0.,-1.));
#4788=DIRECTION('',(1.,0.,0.));
#4789=DIRECTION('center_axis',(1.,0.,0.));
#4790=DIRECTION('ref_axis',(0.,0.,-1.));
#4791=DIRECTION('',(-1.,0.,0.));
#4792=DIRECTION('center_axis',(1.,0.,0.));
#4793=DIRECTION('ref_axis',(0.,0.,-1.));
#4794=DIRECTION('',(1.,0.,0.));
#4795=DIRECTION('center_axis',(-1.,0.,0.));
#4796=DIRECTION('ref_axis',(0.,0.,-1.));
#4797=DIRECTION('center_axis',(1.,0.,0.));
#4798=DIRECTION('ref_axis',(0.,0.,-1.));
#4799=DIRECTION('center_axis',(1.,0.,0.));
#4800=DIRECTION('ref_axis',(0.,0.,-1.));
#4801=DIRECTION('center_axis',(-1.,0.,0.));
#4802=DIRECTION('ref_axis',(0.,0.,-1.));
#4803=DIRECTION('center_axis',(1.,0.,0.));
#4804=DIRECTION('ref_axis',(0.,0.,-1.));
#4805=DIRECTION('',(1.,0.,0.));
#4806=DIRECTION('center_axis',(1.,0.,0.));
#4807=DIRECTION('ref_axis',(0.,0.,-1.));
#4808=DIRECTION('',(-1.,0.,0.));
#4809=DIRECTION('center_axis',(1.,0.,0.));
#4810=DIRECTION('ref_axis',(0.,0.,-1.));
#4811=DIRECTION('',(1.,0.,0.));
#4812=DIRECTION('center_axis',(-1.,0.,0.));
#4813=DIRECTION('ref_axis',(0.,0.,-1.));
#4814=DIRECTION('center_axis',(1.,0.,0.));
#4815=DIRECTION('ref_axis',(0.,0.,-1.));
#4816=DIRECTION('center_axis',(1.,0.,0.));
#4817=DIRECTION('ref_axis',(0.,0.,-1.));
#4818=DIRECTION('center_axis',(-1.,0.,0.));
#4819=DIRECTION('ref_axis',(0.,0.,-1.));
#4820=DIRECTION('center_axis',(1.,0.,0.));
#4821=DIRECTION('ref_axis',(0.,0.,-1.));
#4822=DIRECTION('center_axis',(1.,0.,0.));
#4823=DIRECTION('ref_axis',(0.,0.,-1.));
#4824=DIRECTION('center_axis',(-1.,0.,0.));
#4825=DIRECTION('ref_axis',(0.,0.,-1.));
#4826=DIRECTION('center_axis',(-1.,0.,0.));
#4827=DIRECTION('ref_axis',(0.,0.,-1.));
#4828=DIRECTION('center_axis',(-1.,0.,0.));
#4829=DIRECTION('ref_axis',(0.,0.,-1.));
#4830=DIRECTION('center_axis',(1.,0.,0.));
#4831=DIRECTION('ref_axis',(0.,0.,-1.));
#4832=DIRECTION('center_axis',(1.,0.,0.));
#4833=DIRECTION('ref_axis',(0.,0.,-1.));
#4834=DIRECTION('center_axis',(1.,0.,0.));
#4835=DIRECTION('ref_axis',(0.,0.,-1.));
#4836=DIRECTION('center_axis',(1.,0.,0.));
#4837=DIRECTION('ref_axis',(0.,0.,-1.));
#4838=DIRECTION('center_axis',(1.,0.,0.));
#4839=DIRECTION('ref_axis',(0.,0.,-1.));
#4840=DIRECTION('center_axis',(1.,0.,0.));
#4841=DIRECTION('ref_axis',(0.,0.,-1.));
#4842=DIRECTION('',(1.,0.,0.));
#4843=DIRECTION('center_axis',(-1.,0.,0.));
#4844=DIRECTION('ref_axis',(0.,0.,-1.));
#4845=DIRECTION('',(-1.,0.,0.));
#4846=DIRECTION('',(1.,0.,0.));
#4847=DIRECTION('center_axis',(-1.,0.,0.));
#4848=DIRECTION('ref_axis',(0.,0.,-1.));
#4849=DIRECTION('center_axis',(1.,0.,0.));
#4850=DIRECTION('ref_axis',(0.,0.,-1.));
#4851=DIRECTION('center_axis',(1.,0.,0.));
#4852=DIRECTION('ref_axis',(0.,0.,-1.));
#4853=DIRECTION('center_axis',(1.,0.,0.));
#4854=DIRECTION('ref_axis',(0.,0.,-1.));
#4855=DIRECTION('center_axis',(1.,0.,0.));
#4856=DIRECTION('ref_axis',(0.,0.,-1.));
#4857=DIRECTION('center_axis',(1.,0.,0.));
#4858=DIRECTION('ref_axis',(0.,0.,-1.));
#4859=DIRECTION('',(1.,0.,0.));
#4860=DIRECTION('center_axis',(-1.,0.,0.));
#4861=DIRECTION('ref_axis',(0.,0.,-1.));
#4862=DIRECTION('',(-1.,0.,0.));
#4863=DIRECTION('',(1.,0.,0.));
#4864=DIRECTION('center_axis',(-1.,0.,0.));
#4865=DIRECTION('ref_axis',(0.,0.,-1.));
#4866=DIRECTION('center_axis',(1.,0.,0.));
#4867=DIRECTION('ref_axis',(0.,0.,-1.));
#4868=DIRECTION('center_axis',(1.,0.,0.));
#4869=DIRECTION('ref_axis',(0.,0.,-1.));
#4870=DIRECTION('center_axis',(1.,0.,0.));
#4871=DIRECTION('ref_axis',(0.,0.,-1.));
#4872=DIRECTION('center_axis',(1.,0.,0.));
#4873=DIRECTION('ref_axis',(0.,0.,-1.));
#4874=DIRECTION('center_axis',(1.,0.,0.));
#4875=DIRECTION('ref_axis',(0.,0.,-1.));
#4876=DIRECTION('',(1.,0.,0.));
#4877=DIRECTION('center_axis',(-1.,0.,0.));
#4878=DIRECTION('ref_axis',(0.,0.,-1.));
#4879=DIRECTION('',(-1.,0.,0.));
#4880=DIRECTION('',(1.,0.,0.));
#4881=DIRECTION('center_axis',(-1.,0.,0.));
#4882=DIRECTION('ref_axis',(0.,0.,-1.));
#4883=DIRECTION('center_axis',(1.,0.,0.));
#4884=DIRECTION('ref_axis',(0.,0.,-1.));
#4885=DIRECTION('',(-1.,0.,0.));
#4886=DIRECTION('center_axis',(1.,0.,0.));
#4887=DIRECTION('ref_axis',(0.,0.,-1.));
#4888=DIRECTION('center_axis',(1.,0.,0.));
#4889=DIRECTION('ref_axis',(0.,0.,-1.));
#4890=DIRECTION('center_axis',(1.,0.,0.));
#4891=DIRECTION('ref_axis',(0.,0.,-1.));
#4892=DIRECTION('center_axis',(1.,0.,0.));
#4893=DIRECTION('ref_axis',(0.,0.,-1.));
#4894=DIRECTION('center_axis',(1.,0.,0.));
#4895=DIRECTION('ref_axis',(0.,0.,-1.));
#4896=DIRECTION('',(-1.,0.,0.));
#4897=DIRECTION('center_axis',(1.,0.,0.));
#4898=DIRECTION('ref_axis',(0.,0.,-1.));
#4899=DIRECTION('center_axis',(1.,0.,0.));
#4900=DIRECTION('ref_axis',(0.,0.,-1.));
#4901=DIRECTION('center_axis',(1.,0.,0.));
#4902=DIRECTION('ref_axis',(0.,0.,-1.));
#4903=DIRECTION('',(-1.,0.,0.));
#4904=DIRECTION('center_axis',(1.,0.,0.));
#4905=DIRECTION('ref_axis',(0.,0.,-1.));
#4906=DIRECTION('center_axis',(1.,0.,0.));
#4907=DIRECTION('ref_axis',(0.,0.,-1.));
#4908=DIRECTION('center_axis',(-1.,0.,0.));
#4909=DIRECTION('ref_axis',(0.,0.,-1.));
#4910=DIRECTION('',(-1.,0.,0.));
#4911=DIRECTION('center_axis',(-1.,0.,0.));
#4912=DIRECTION('ref_axis',(0.,0.,-1.));
#4913=DIRECTION('center_axis',(1.,0.,0.));
#4914=DIRECTION('ref_axis',(0.,0.,-1.));
#4915=DIRECTION('center_axis',(1.,0.,0.));
#4916=DIRECTION('ref_axis',(0.,0.,-1.));
#4917=DIRECTION('axis',(0.,0.,1.));
#4918=DIRECTION('refdir',(1.,0.,0.));
#4919=DIRECTION('center_axis',(0.,0.,1.));
#4920=DIRECTION('ref_axis',(1.,0.,0.));
#4921=DIRECTION('center_axis',(0.,0.,1.));
#4922=DIRECTION('ref_axis',(1.,0.,0.));
#4923=DIRECTION('',(0.,0.,1.));
#4924=DIRECTION('center_axis',(0.,0.,-1.));
#4925=DIRECTION('ref_axis',(1.,0.,0.));
#4926=DIRECTION('center_axis',(0.,0.,1.));
#4927=DIRECTION('ref_axis',(1.,0.,0.));
#4928=DIRECTION('center_axis',(0.,0.,1.));
#4929=DIRECTION('ref_axis',(1.,0.,0.));
#4930=DIRECTION('center_axis',(0.,0.,1.));
#4931=DIRECTION('ref_axis',(1.,0.,0.));
#4932=DIRECTION('',(0.,0.,1.));
#4933=DIRECTION('center_axis',(0.,0.,-1.));
#4934=DIRECTION('ref_axis',(1.,0.,0.));
#4935=DIRECTION('center_axis',(0.,0.,1.));
#4936=DIRECTION('ref_axis',(1.,0.,0.));
#4937=DIRECTION('center_axis',(0.,0.,1.));
#4938=DIRECTION('ref_axis',(1.,0.,0.));
#4939=DIRECTION('center_axis',(0.,0.,1.));
#4940=DIRECTION('ref_axis',(1.,0.,0.));
#4941=DIRECTION('',(0.,0.,1.));
#4942=DIRECTION('center_axis',(0.,0.,1.));
#4943=DIRECTION('ref_axis',(1.,0.,0.));
#4944=DIRECTION('center_axis',(0.,0.,1.));
#4945=DIRECTION('ref_axis',(1.,0.,0.));
#4946=DIRECTION('center_axis',(0.,0.,1.));
#4947=DIRECTION('ref_axis',(1.,0.,0.));
#4948=DIRECTION('center_axis',(0.,0.,1.));
#4949=DIRECTION('ref_axis',(1.,0.,0.));
#4950=DIRECTION('',(0.,0.,1.));
#4951=DIRECTION('center_axis',(0.,0.,1.));
#4952=DIRECTION('ref_axis',(1.,0.,0.));
#4953=DIRECTION('center_axis',(0.,0.,1.));
#4954=DIRECTION('ref_axis',(1.,0.,0.));
#4955=DIRECTION('center_axis',(1.,0.,0.));
#4956=DIRECTION('ref_axis',(0.,0.,-1.));
#4957=DIRECTION('center_axis',(1.,0.,0.));
#4958=DIRECTION('ref_axis',(0.,0.,-1.));
#4959=DIRECTION('',(-1.,0.,0.));
#4960=DIRECTION('center_axis',(-1.,0.,0.));
#4961=DIRECTION('ref_axis',(0.,0.,-1.));
#4962=DIRECTION('',(1.,0.,0.));
#4963=DIRECTION('center_axis',(1.,0.,0.));
#4964=DIRECTION('ref_axis',(0.,1.,0.));
#4965=DIRECTION('',(0.,1.,0.));
#4966=DIRECTION('',(0.,0.,1.));
#4967=DIRECTION('',(0.,1.,0.));
#4968=DIRECTION('',(0.,0.,1.));
#4969=DIRECTION('',(0.,1.,0.));
#4970=DIRECTION('center_axis',(0.,0.,1.));
#4971=DIRECTION('ref_axis',(1.,0.,0.));
#4972=DIRECTION('',(0.,-1.,0.));
#4973=DIRECTION('',(1.,0.,0.));
#4974=DIRECTION('center_axis',(0.,1.,0.));
#4975=DIRECTION('ref_axis',(-1.,0.,0.));
#4976=DIRECTION('',(-1.,0.,0.));
#4977=DIRECTION('',(0.,0.,1.));
#4978=DIRECTION('',(-1.,0.,0.));
#4979=DIRECTION('center_axis',(0.,-1.,0.));
#4980=DIRECTION('ref_axis',(1.,0.,0.));
#4981=DIRECTION('',(1.,0.,0.));
#4982=DIRECTION('',(0.,0.,1.));
#4983=DIRECTION('center_axis',(-1.,0.,0.));
#4984=DIRECTION('ref_axis',(0.,-1.,0.));
#4985=DIRECTION('',(0.,-1.,0.));
#4986=DIRECTION('',(0.,-1.,0.));
#4987=DIRECTION('center_axis',(0.,0.,1.));
#4988=DIRECTION('ref_axis',(1.,0.,0.));
#4989=DIRECTION('center_axis',(0.,0.,1.));
#4990=DIRECTION('ref_axis',(1.,0.,0.));
#4991=DIRECTION('axis',(0.,0.,1.));
#4992=DIRECTION('refdir',(1.,0.,0.));
#4993=DIRECTION('center_axis',(0.,0.,1.));
#4994=DIRECTION('ref_axis',(1.,0.,0.));
#4995=DIRECTION('',(-1.,0.,0.));
#4996=DIRECTION('center_axis',(0.,0.,1.));
#4997=DIRECTION('ref_axis',(1.,0.,0.));
#4998=DIRECTION('center_axis',(0.,0.,1.));
#4999=DIRECTION('ref_axis',(1.,0.,0.));
#5000=DIRECTION('center_axis',(0.,0.,1.));
#5001=DIRECTION('ref_axis',(2.83276944882399E-16,1.,0.));
#5002=DIRECTION('',(0.,0.,-1.));
#5003=DIRECTION('center_axis',(0.,0.,-1.));
#5004=DIRECTION('ref_axis',(1.,0.,0.));
#5005=DIRECTION('',(0.,0.,1.));
#5006=DIRECTION('center_axis',(0.,0.,1.));
#5007=DIRECTION('ref_axis',(1.,0.,0.));
#5008=DIRECTION('',(1.,0.,0.));
#5009=DIRECTION('center_axis',(0.,0.,1.));
#5010=DIRECTION('ref_axis',(1.,0.,0.));
#5011=DIRECTION('center_axis',(0.,0.,1.));
#5012=DIRECTION('ref_axis',(1.,0.,0.));
#5013=DIRECTION('center_axis',(0.,0.,1.));
#5014=DIRECTION('ref_axis',(-1.83697019872103E-16,-1.,0.));
#5015=DIRECTION('',(0.,0.,-1.));
#5016=DIRECTION('center_axis',(0.,0.,-1.));
#5017=DIRECTION('ref_axis',(1.,0.,0.));
#5018=DIRECTION('',(0.,0.,1.));
#5019=DIRECTION('center_axis',(0.,-1.,0.));
#5020=DIRECTION('ref_axis',(1.,0.,0.));
#5021=DIRECTION('',(1.,0.,0.));
#5022=DIRECTION('',(0.,0.,1.));
#5023=DIRECTION('',(1.,0.,0.));
#5024=DIRECTION('',(0.,0.,1.));
#5025=DIRECTION('',(1.,0.,0.));
#5026=DIRECTION('center_axis',(0.,1.,0.));
#5027=DIRECTION('ref_axis',(-1.,0.,0.));
#5028=DIRECTION('',(-1.,0.,0.));
#5029=DIRECTION('',(0.,0.,1.));
#5030=DIRECTION('',(-1.,0.,0.));
#5031=DIRECTION('',(0.,0.,1.));
#5032=DIRECTION('',(-1.,0.,0.));
#5033=DIRECTION('center_axis',(0.,0.,1.));
#5034=DIRECTION('ref_axis',(1.,0.,0.));
#5035=DIRECTION('center_axis',(0.,0.,1.));
#5036=DIRECTION('ref_axis',(1.,0.,0.));
#5037=DIRECTION('',(0.,0.,1.));
#5038=DIRECTION('center_axis',(0.,0.,1.));
#5039=DIRECTION('ref_axis',(1.,0.,0.));
#5040=DIRECTION('center_axis',(0.,0.,1.));
#5041=DIRECTION('ref_axis',(1.,0.,0.));
#5042=DIRECTION('',(0.,0.,1.));
#5043=DIRECTION('center_axis',(1.,0.,0.));
#5044=DIRECTION('ref_axis',(0.,1.22464679914735E-16,1.));
#5045=DIRECTION('center_axis',(1.,0.,0.));
#5046=DIRECTION('ref_axis',(0.,0.,-1.));
#5047=DIRECTION('',(-1.,0.,0.));
#5048=DIRECTION('center_axis',(-1.,0.,0.));
#5049=DIRECTION('ref_axis',(0.,0.,-1.));
#5050=DIRECTION('',(1.,0.,0.));
#5051=DIRECTION('center_axis',(1.,0.,0.));
#5052=DIRECTION('ref_axis',(0.,1.,0.));
#5053=DIRECTION('',(0.,1.,0.));
#5054=DIRECTION('',(0.,1.,0.));
#5055=DIRECTION('',(0.,1.,0.));
#5056=DIRECTION('center_axis',(0.,0.,1.));
#5057=DIRECTION('ref_axis',(1.,0.,0.));
#5058=DIRECTION('',(0.,-1.,0.));
#5059=DIRECTION('center_axis',(-1.,0.,0.));
#5060=DIRECTION('ref_axis',(0.,-1.,0.));
#5061=DIRECTION('',(0.,-1.,0.));
#5062=DIRECTION('',(0.,-1.,0.));
#5063=DIRECTION('center_axis',(0.,0.,1.));
#5064=DIRECTION('ref_axis',(1.,0.,0.));
#5065=DIRECTION('center_axis',(0.,0.,1.));
#5066=DIRECTION('ref_axis',(1.,0.,0.));
#5067=DIRECTION('axis',(0.,0.,1.));
#5068=DIRECTION('refdir',(1.,0.,0.));
#5069=DIRECTION('center_axis',(0.,0.,1.));
#5070=DIRECTION('ref_axis',(1.,0.,0.));
#5071=DIRECTION('center_axis',(0.,0.,1.));
#5072=DIRECTION('ref_axis',(1.,0.,0.));
#5073=DIRECTION('',(0.,0.,1.));
#5074=DIRECTION('center_axis',(0.,0.,-1.));
#5075=DIRECTION('ref_axis',(1.,0.,0.));
#5076=DIRECTION('center_axis',(0.,0.,1.));
#5077=DIRECTION('ref_axis',(1.,0.,0.));
#5078=DIRECTION('center_axis',(0.,0.,1.));
#5079=DIRECTION('ref_axis',(1.,0.,0.));
#5080=DIRECTION('center_axis',(0.,0.,1.));
#5081=DIRECTION('ref_axis',(1.,0.,0.));
#5082=DIRECTION('',(0.,0.,1.));
#5083=DIRECTION('center_axis',(0.,0.,-1.));
#5084=DIRECTION('ref_axis',(1.,0.,0.));
#5085=DIRECTION('center_axis',(0.,0.,1.));
#5086=DIRECTION('ref_axis',(1.,0.,0.));
#5087=DIRECTION('center_axis',(0.,0.,1.));
#5088=DIRECTION('ref_axis',(1.,0.,0.));
#5089=DIRECTION('center_axis',(0.,0.,1.));
#5090=DIRECTION('ref_axis',(1.,0.,0.));
#5091=DIRECTION('',(0.,0.,1.));
#5092=DIRECTION('center_axis',(0.,0.,1.));
#5093=DIRECTION('ref_axis',(1.,0.,0.));
#5094=DIRECTION('center_axis',(0.,0.,1.));
#5095=DIRECTION('ref_axis',(1.,0.,0.));
#5096=DIRECTION('center_axis',(0.,0.,1.));
#5097=DIRECTION('ref_axis',(1.,0.,0.));
#5098=DIRECTION('center_axis',(0.,0.,1.));
#5099=DIRECTION('ref_axis',(1.,0.,0.));
#5100=DIRECTION('',(0.,0.,1.));
#5101=DIRECTION('center_axis',(0.,0.,1.));
#5102=DIRECTION('ref_axis',(1.,0.,0.));
#5103=DIRECTION('center_axis',(0.,0.,1.));
#5104=DIRECTION('ref_axis',(1.,0.,0.));
#5105=DIRECTION('center_axis',(1.,0.,0.));
#5106=DIRECTION('ref_axis',(0.,0.,-1.));
#5107=DIRECTION('center_axis',(1.,0.,0.));
#5108=DIRECTION('ref_axis',(0.,0.,-1.));
#5109=DIRECTION('',(-1.,0.,0.));
#5110=DIRECTION('center_axis',(-1.,0.,0.));
#5111=DIRECTION('ref_axis',(0.,0.,-1.));
#5112=DIRECTION('',(1.,0.,0.));
#5113=DIRECTION('center_axis',(1.,0.,0.));
#5114=DIRECTION('ref_axis',(0.,1.,0.));
#5115=DIRECTION('',(0.,1.,0.));
#5116=DIRECTION('',(0.,0.,1.));
#5117=DIRECTION('',(0.,1.,0.));
#5118=DIRECTION('',(0.,0.,1.));
#5119=DIRECTION('',(0.,1.,0.));
#5120=DIRECTION('center_axis',(0.,0.,1.));
#5121=DIRECTION('ref_axis',(1.,0.,0.));
#5122=DIRECTION('',(0.,-1.,0.));
#5123=DIRECTION('',(1.,0.,0.));
#5124=DIRECTION('center_axis',(0.,1.,0.));
#5125=DIRECTION('ref_axis',(-1.,0.,0.));
#5126=DIRECTION('',(-1.,0.,0.));
#5127=DIRECTION('',(0.,0.,1.));
#5128=DIRECTION('',(-1.,0.,0.));
#5129=DIRECTION('center_axis',(0.,-1.,0.));
#5130=DIRECTION('ref_axis',(1.,0.,0.));
#5131=DIRECTION('',(1.,0.,0.));
#5132=DIRECTION('',(0.,0.,1.));
#5133=DIRECTION('center_axis',(-1.,0.,0.));
#5134=DIRECTION('ref_axis',(0.,-1.,0.));
#5135=DIRECTION('',(0.,-1.,0.));
#5136=DIRECTION('',(0.,-1.,0.));
#5137=DIRECTION('center_axis',(0.,0.,1.));
#5138=DIRECTION('ref_axis',(1.,0.,0.));
#5139=DIRECTION('center_axis',(0.,0.,1.));
#5140=DIRECTION('ref_axis',(1.,0.,0.));
#5141=DIRECTION('axis',(0.,0.,1.));
#5142=DIRECTION('refdir',(1.,0.,0.));
#5143=DIRECTION('center_axis',(0.,0.,1.));
#5144=DIRECTION('ref_axis',(1.,0.,0.));
#5145=DIRECTION('',(-1.,0.,0.));
#5146=DIRECTION('center_axis',(0.,0.,1.));
#5147=DIRECTION('ref_axis',(1.,0.,0.));
#5148=DIRECTION('center_axis',(0.,0.,1.));
#5149=DIRECTION('ref_axis',(1.,0.,0.));
#5150=DIRECTION('center_axis',(0.,0.,1.));
#5151=DIRECTION('ref_axis',(5.0532154980743E-16,1.,0.));
#5152=DIRECTION('',(0.,0.,-1.));
#5153=DIRECTION('center_axis',(0.,0.,-1.));
#5154=DIRECTION('ref_axis',(1.,0.,0.));
#5155=DIRECTION('',(0.,0.,1.));
#5156=DIRECTION('center_axis',(0.,0.,1.));
#5157=DIRECTION('ref_axis',(1.,0.,0.));
#5158=DIRECTION('',(1.,0.,0.));
#5159=DIRECTION('center_axis',(0.,0.,1.));
#5160=DIRECTION('ref_axis',(1.,0.,0.));
#5161=DIRECTION('center_axis',(0.,0.,1.));
#5162=DIRECTION('ref_axis',(1.,0.,0.));
#5163=DIRECTION('center_axis',(0.,0.,1.));
#5164=DIRECTION('ref_axis',(-1.83697019872103E-16,-1.,0.));
#5165=DIRECTION('',(0.,0.,-1.));
#5166=DIRECTION('center_axis',(0.,0.,-1.));
#5167=DIRECTION('ref_axis',(1.,0.,0.));
#5168=DIRECTION('',(0.,0.,1.));
#5169=DIRECTION('center_axis',(0.,-1.,0.));
#5170=DIRECTION('ref_axis',(1.,0.,0.));
#5171=DIRECTION('',(1.,0.,0.));
#5172=DIRECTION('',(0.,0.,1.));
#5173=DIRECTION('',(1.,0.,0.));
#5174=DIRECTION('',(0.,0.,1.));
#5175=DIRECTION('',(1.,0.,0.));
#5176=DIRECTION('center_axis',(0.,1.,0.));
#5177=DIRECTION('ref_axis',(-1.,0.,0.));
#5178=DIRECTION('',(-1.,0.,0.));
#5179=DIRECTION('',(0.,0.,1.));
#5180=DIRECTION('',(-1.,0.,0.));
#5181=DIRECTION('',(0.,0.,1.));
#5182=DIRECTION('',(-1.,0.,0.));
#5183=DIRECTION('center_axis',(0.,0.,1.));
#5184=DIRECTION('ref_axis',(1.,0.,0.));
#5185=DIRECTION('center_axis',(0.,0.,1.));
#5186=DIRECTION('ref_axis',(1.,0.,0.));
#5187=DIRECTION('',(0.,0.,1.));
#5188=DIRECTION('center_axis',(0.,0.,1.));
#5189=DIRECTION('ref_axis',(1.,0.,0.));
#5190=DIRECTION('center_axis',(0.,0.,1.));
#5191=DIRECTION('ref_axis',(1.,0.,0.));
#5192=DIRECTION('',(0.,0.,1.));
#5193=DIRECTION('center_axis',(1.,0.,0.));
#5194=DIRECTION('ref_axis',(0.,1.22464679914735E-16,1.));
#5195=DIRECTION('center_axis',(1.,0.,0.));
#5196=DIRECTION('ref_axis',(0.,0.,-1.));
#5197=DIRECTION('',(-1.,0.,0.));
#5198=DIRECTION('center_axis',(-1.,0.,0.));
#5199=DIRECTION('ref_axis',(0.,0.,-1.));
#5200=DIRECTION('',(1.,0.,0.));
#5201=DIRECTION('center_axis',(1.,0.,0.));
#5202=DIRECTION('ref_axis',(0.,1.,0.));
#5203=DIRECTION('',(0.,1.,0.));
#5204=DIRECTION('',(0.,1.,0.));
#5205=DIRECTION('',(0.,1.,0.));
#5206=DIRECTION('center_axis',(0.,0.,1.));
#5207=DIRECTION('ref_axis',(1.,0.,0.));
#5208=DIRECTION('',(0.,-1.,0.));
#5209=DIRECTION('center_axis',(-1.,0.,0.));
#5210=DIRECTION('ref_axis',(0.,-1.,0.));
#5211=DIRECTION('',(0.,-1.,0.));
#5212=DIRECTION('',(0.,-1.,0.));
#5213=DIRECTION('center_axis',(0.,0.,1.));
#5214=DIRECTION('ref_axis',(1.,0.,0.));
#5215=DIRECTION('center_axis',(0.,0.,1.));
#5216=DIRECTION('ref_axis',(1.,0.,0.));
#5217=DIRECTION('axis',(0.,0.,1.));
#5218=DIRECTION('refdir',(1.,0.,0.));
#5219=DIRECTION('center_axis',(1.,0.,0.));
#5220=DIRECTION('ref_axis',(0.,0.,-1.));
#5221=DIRECTION('center_axis',(-1.,0.,0.));
#5222=DIRECTION('ref_axis',(0.,0.,-1.));
#5223=DIRECTION('',(-1.,0.,0.));
#5224=DIRECTION('center_axis',(-1.,0.,0.));
#5225=DIRECTION('ref_axis',(0.,0.,-1.));
#5226=DIRECTION('center_axis',(1.,0.,0.));
#5227=DIRECTION('ref_axis',(0.,0.,-1.));
#5228=DIRECTION('center_axis',(1.,0.,0.));
#5229=DIRECTION('ref_axis',(0.,0.,-1.));
#5230=DIRECTION('',(-1.,0.,0.));
#5231=DIRECTION('center_axis',(1.,0.,0.));
#5232=DIRECTION('ref_axis',(0.,0.,-1.));
#5233=DIRECTION('center_axis',(1.,0.,0.));
#5234=DIRECTION('ref_axis',(0.,0.,-1.));
#5235=DIRECTION('center_axis',(1.,0.,0.));
#5236=DIRECTION('ref_axis',(0.,0.,-1.));
#5237=DIRECTION('axis',(0.,0.,1.));
#5238=DIRECTION('refdir',(1.,0.,0.));
#5239=DIRECTION('center_axis',(1.,0.,0.));
#5240=DIRECTION('ref_axis',(0.,0.,-1.));
#5241=DIRECTION('center_axis',(-1.,0.,0.));
#5242=DIRECTION('ref_axis',(0.,0.,-1.));
#5243=DIRECTION('',(-1.,0.,0.));
#5244=DIRECTION('center_axis',(-1.,0.,0.));
#5245=DIRECTION('ref_axis',(0.,0.,-1.));
#5246=DIRECTION('center_axis',(1.,0.,0.));
#5247=DIRECTION('ref_axis',(0.,0.,-1.));
#5248=DIRECTION('center_axis',(1.,0.,0.));
#5249=DIRECTION('ref_axis',(0.,0.,-1.));
#5250=DIRECTION('',(-1.,0.,0.));
#5251=DIRECTION('center_axis',(1.,0.,0.));
#5252=DIRECTION('ref_axis',(0.,0.,-1.));
#5253=DIRECTION('center_axis',(1.,0.,0.));
#5254=DIRECTION('ref_axis',(0.,0.,-1.));
#5255=DIRECTION('center_axis',(1.,0.,0.));
#5256=DIRECTION('ref_axis',(0.,0.,-1.));
#5257=DIRECTION('axis',(0.,0.,1.));
#5258=DIRECTION('refdir',(1.,0.,0.));
#5259=DIRECTION('center_axis',(1.,0.,0.));
#5260=DIRECTION('ref_axis',(0.,0.,-1.));
#5261=DIRECTION('center_axis',(-1.,0.,0.));
#5262=DIRECTION('ref_axis',(0.,0.,-1.));
#5263=DIRECTION('',(-1.,0.,0.));
#5264=DIRECTION('center_axis',(-1.,0.,0.));
#5265=DIRECTION('ref_axis',(0.,0.,-1.));
#5266=DIRECTION('center_axis',(1.,0.,0.));
#5267=DIRECTION('ref_axis',(0.,0.,-1.));
#5268=DIRECTION('center_axis',(1.,0.,0.));
#5269=DIRECTION('ref_axis',(0.,0.,-1.));
#5270=DIRECTION('',(-1.,0.,0.));
#5271=DIRECTION('center_axis',(1.,0.,0.));
#5272=DIRECTION('ref_axis',(0.,0.,-1.));
#5273=DIRECTION('center_axis',(1.,0.,0.));
#5274=DIRECTION('ref_axis',(0.,0.,-1.));
#5275=DIRECTION('center_axis',(1.,0.,0.));
#5276=DIRECTION('ref_axis',(0.,0.,-1.));
#5277=DIRECTION('axis',(0.,0.,1.));
#5278=DIRECTION('refdir',(1.,0.,0.));
#5279=DIRECTION('center_axis',(1.,0.,0.));
#5280=DIRECTION('ref_axis',(0.,0.,-1.));
#5281=DIRECTION('center_axis',(1.,0.,0.));
#5282=DIRECTION('ref_axis',(0.,0.,-1.));
#5283=DIRECTION('',(1.,0.,0.));
#5284=DIRECTION('center_axis',(-1.,0.,0.));
#5285=DIRECTION('ref_axis',(0.,0.,-1.));
#5286=DIRECTION('center_axis',(1.,0.,0.));
#5287=DIRECTION('ref_axis',(0.,0.,-1.));
#5288=DIRECTION('center_axis',(1.,0.,0.));
#5289=DIRECTION('ref_axis',(0.,0.,-1.));
#5290=DIRECTION('',(1.,0.,0.));
#5291=DIRECTION('center_axis',(-1.,0.,0.));
#5292=DIRECTION('ref_axis',(0.,0.,-1.));
#5293=DIRECTION('center_axis',(1.,0.,0.));
#5294=DIRECTION('ref_axis',(0.,0.,-1.));
#5295=DIRECTION('center_axis',(1.,0.,0.));
#5296=DIRECTION('ref_axis',(0.,0.,-1.));
#5297=DIRECTION('',(1.,0.,0.));
#5298=DIRECTION('center_axis',(-1.,0.,0.));
#5299=DIRECTION('ref_axis',(0.,0.,-1.));
#5300=DIRECTION('center_axis',(1.,0.,0.));
#5301=DIRECTION('ref_axis',(0.,0.,-1.));
#5302=DIRECTION('center_axis',(1.,0.,0.));
#5303=DIRECTION('ref_axis',(0.,0.,-1.));
#5304=DIRECTION('',(-1.,0.,0.));
#5305=DIRECTION('center_axis',(1.,0.,0.));
#5306=DIRECTION('ref_axis',(0.,0.,-1.));
#5307=DIRECTION('center_axis',(1.,0.,0.));
#5308=DIRECTION('ref_axis',(0.,0.,-1.));
#5309=DIRECTION('center_axis',(-1.,0.,0.));
#5310=DIRECTION('ref_axis',(0.,0.,-1.));
#5311=DIRECTION('center_axis',(1.,0.,0.));
#5312=DIRECTION('ref_axis',(0.,0.,-1.));
#5313=DIRECTION('center_axis',(-1.,0.,0.));
#5314=DIRECTION('ref_axis',(0.,0.,-1.));
#5315=DIRECTION('',(-1.,0.,0.));
#5316=DIRECTION('center_axis',(1.,0.,0.));
#5317=DIRECTION('ref_axis',(0.,0.,-1.));
#5318=DIRECTION('center_axis',(1.,0.,0.));
#5319=DIRECTION('ref_axis',(0.,0.,-1.));
#5320=DIRECTION('',(-1.,0.,0.));
#5321=DIRECTION('center_axis',(1.,0.,0.));
#5322=DIRECTION('ref_axis',(0.,0.,-1.));
#5323=DIRECTION('center_axis',(1.,0.,0.));
#5324=DIRECTION('ref_axis',(0.,0.,-1.));
#5325=DIRECTION('center_axis',(1.,0.,0.));
#5326=DIRECTION('ref_axis',(0.,0.,-1.));
#5327=DIRECTION('axis',(0.,0.,1.));
#5328=DIRECTION('refdir',(1.,0.,0.));
#5329=DIRECTION('center_axis',(0.,0.,1.));
#5330=DIRECTION('ref_axis',(1.,0.,0.));
#5331=DIRECTION('',(-1.,0.,0.));
#5332=DIRECTION('center_axis',(0.,0.,1.));
#5333=DIRECTION('ref_axis',(1.,0.,0.));
#5334=DIRECTION('center_axis',(0.,0.,1.));
#5335=DIRECTION('ref_axis',(1.,0.,0.));
#5336=DIRECTION('center_axis',(0.,0.,1.));
#5337=DIRECTION('ref_axis',(1.,0.,0.));
#5338=DIRECTION('',(0.,0.,1.));
#5339=DIRECTION('center_axis',(0.,0.,1.));
#5340=DIRECTION('ref_axis',(1.,0.,0.));
#5341=DIRECTION('',(0.,0.,1.));
#5342=DIRECTION('center_axis',(0.,0.,-1.));
#5343=DIRECTION('ref_axis',(1.,0.,0.));
#5344=DIRECTION('center_axis',(1.,0.,0.));
#5345=DIRECTION('ref_axis',(0.,0.,-1.));
#5346=DIRECTION('center_axis',(1.,0.,0.));
#5347=DIRECTION('ref_axis',(0.,0.,-1.));
#5348=DIRECTION('center_axis',(1.,0.,0.));
#5349=DIRECTION('ref_axis',(0.,0.,-1.));
#5350=DIRECTION('center_axis',(1.,0.,0.));
#5351=DIRECTION('ref_axis',(0.,0.,-1.));
#5352=DIRECTION('center_axis',(1.,0.,0.));
#5353=DIRECTION('ref_axis',(0.,0.,-1.));
#5354=DIRECTION('',(1.,0.,0.));
#5355=DIRECTION('center_axis',(-1.,0.,0.));
#5356=DIRECTION('ref_axis',(0.,0.,-1.));
#5357=DIRECTION('',(-1.,0.,0.));
#5358=DIRECTION('',(1.,0.,0.));
#5359=DIRECTION('center_axis',(-1.,0.,0.));
#5360=DIRECTION('ref_axis',(0.,0.,-1.));
#5361=DIRECTION('center_axis',(1.,0.,0.));
#5362=DIRECTION('ref_axis',(0.,0.,-1.));
#5363=DIRECTION('center_axis',(1.,0.,0.));
#5364=DIRECTION('ref_axis',(0.,0.,-1.));
#5365=DIRECTION('center_axis',(1.,0.,0.));
#5366=DIRECTION('ref_axis',(0.,0.,-1.));
#5367=DIRECTION('center_axis',(1.,0.,0.));
#5368=DIRECTION('ref_axis',(0.,0.,-1.));
#5369=DIRECTION('center_axis',(1.,0.,0.));
#5370=DIRECTION('ref_axis',(0.,0.,-1.));
#5371=DIRECTION('',(1.,0.,0.));
#5372=DIRECTION('center_axis',(-1.,0.,0.));
#5373=DIRECTION('ref_axis',(0.,0.,-1.));
#5374=DIRECTION('',(-1.,0.,0.));
#5375=DIRECTION('',(1.,0.,0.));
#5376=DIRECTION('center_axis',(-1.,0.,0.));
#5377=DIRECTION('ref_axis',(0.,0.,-1.));
#5378=DIRECTION('center_axis',(1.,0.,0.));
#5379=DIRECTION('ref_axis',(0.,0.,-1.));
#5380=DIRECTION('center_axis',(1.,0.,0.));
#5381=DIRECTION('ref_axis',(0.,0.,-1.));
#5382=DIRECTION('center_axis',(1.,0.,0.));
#5383=DIRECTION('ref_axis',(0.,0.,-1.));
#5384=DIRECTION('center_axis',(1.,0.,0.));
#5385=DIRECTION('ref_axis',(0.,0.,-1.));
#5386=DIRECTION('center_axis',(1.,0.,0.));
#5387=DIRECTION('ref_axis',(0.,0.,-1.));
#5388=DIRECTION('',(1.,0.,0.));
#5389=DIRECTION('center_axis',(-1.,0.,0.));
#5390=DIRECTION('ref_axis',(0.,0.,-1.));
#5391=DIRECTION('',(-1.,0.,0.));
#5392=DIRECTION('',(1.,0.,0.));
#5393=DIRECTION('center_axis',(-1.,0.,0.));
#5394=DIRECTION('ref_axis',(0.,0.,-1.));
#5395=DIRECTION('center_axis',(1.,0.,0.));
#5396=DIRECTION('ref_axis',(0.,-1.,1.83697019872103E-16));
#5397=DIRECTION('center_axis',(-1.,0.,0.));
#5398=DIRECTION('ref_axis',(0.,0.,-1.));
#5399=DIRECTION('center_axis',(-1.,0.,0.));
#5400=DIRECTION('ref_axis',(0.,0.,-1.));
#5401=DIRECTION('center_axis',(-1.,0.,0.));
#5402=DIRECTION('ref_axis',(0.,0.,-1.));
#5403=DIRECTION('',(1.,0.,0.));
#5404=DIRECTION('center_axis',(1.,0.,0.));
#5405=DIRECTION('ref_axis',(0.,0.,-1.));
#5406=DIRECTION('',(-1.,0.,0.));
#5407=DIRECTION('center_axis',(-1.,0.,0.));
#5408=DIRECTION('ref_axis',(0.,0.,-1.));
#5409=DIRECTION('center_axis',(0.,0.,1.));
#5410=DIRECTION('ref_axis',(0.,-1.,0.));
#5411=DIRECTION('',(1.,0.,0.));
#5412=DIRECTION('',(0.,-1.,0.));
#5413=DIRECTION('',(0.,1.,0.));
#5414=DIRECTION('center_axis',(0.,0.,-1.));
#5415=DIRECTION('ref_axis',(0.,1.,0.));
#5416=DIRECTION('',(-1.,0.,0.));
#5417=DIRECTION('',(0.,-1.,0.));
#5418=DIRECTION('',(0.,1.,0.));
#5419=DIRECTION('center_axis',(1.,0.,0.));
#5420=DIRECTION('ref_axis',(0.,0.,-1.));
#5421=DIRECTION('center_axis',(1.,0.,0.));
#5422=DIRECTION('ref_axis',(0.,0.,-1.));
#5423=DIRECTION('center_axis',(1.,0.,0.));
#5424=DIRECTION('ref_axis',(0.,0.,-1.));
#5425=DIRECTION('center_axis',(1.,0.,0.));
#5426=DIRECTION('ref_axis',(0.,0.,-1.));
#5427=DIRECTION('center_axis',(-1.,0.,0.));
#5428=DIRECTION('ref_axis',(0.,0.,-1.));
#5429=DIRECTION('center_axis',(-1.,0.,0.));
#5430=DIRECTION('ref_axis',(0.,0.,-1.));
#5431=DIRECTION('center_axis',(1.,0.,0.));
#5432=DIRECTION('ref_axis',(0.,0.,-1.));
#5433=DIRECTION('',(-1.,0.,0.));
#5434=DIRECTION('center_axis',(-1.,0.,0.));
#5435=DIRECTION('ref_axis',(0.,0.,-1.));
#5436=DIRECTION('center_axis',(1.,0.,0.));
#5437=DIRECTION('ref_axis',(0.,0.,-1.));
#5438=DIRECTION('',(-1.,0.,0.));
#5439=DIRECTION('center_axis',(1.,0.,0.));
#5440=DIRECTION('ref_axis',(0.,0.,-1.));
#5441=DIRECTION('center_axis',(1.,0.,0.));
#5442=DIRECTION('ref_axis',(0.,0.,-1.));
#5443=DIRECTION('axis',(0.,0.,1.));
#5444=DIRECTION('refdir',(1.,0.,0.));
#5445=DIRECTION('center_axis',(0.,1.,0.));
#5446=DIRECTION('ref_axis',(0.,0.,1.));
#5447=DIRECTION('center_axis',(0.,-1.,0.));
#5448=DIRECTION('ref_axis',(1.,0.,0.));
#5449=DIRECTION('center_axis',(0.,-1.,0.));
#5450=DIRECTION('ref_axis',(1.,0.,0.));
#5451=DIRECTION('center_axis',(0.,-1.,0.));
#5452=DIRECTION('ref_axis',(1.,0.,0.));
#5453=DIRECTION('',(0.707106781186548,0.707106781186547,8.65956056235493E-17));
#5454=DIRECTION('center_axis',(0.,-1.,0.));
#5455=DIRECTION('ref_axis',(1.,0.,0.));
#5456=DIRECTION('center_axis',(0.,-1.,0.));
#5457=DIRECTION('ref_axis',(1.,0.,0.));
#5458=DIRECTION('',(0.,1.,0.));
#5459=DIRECTION('center_axis',(0.,1.,0.));
#5460=DIRECTION('ref_axis',(1.,0.,0.));
#5461=DIRECTION('center_axis',(0.,-1.,0.));
#5462=DIRECTION('ref_axis',(1.,0.,0.));
#5463=DIRECTION('',(-0.707106781186547,0.707106781186548,-8.65956056235493E-17));
#5464=DIRECTION('center_axis',(0.,-1.,0.));
#5465=DIRECTION('ref_axis',(0.,0.,-1.));
#5466=DIRECTION('center_axis',(0.,-1.,0.));
#5467=DIRECTION('ref_axis',(1.,0.,0.));
#5468=DIRECTION('center_axis',(0.,1.,0.));
#5469=DIRECTION('ref_axis',(1.,0.,0.));
#5470=DIRECTION('center_axis',(0.,1.,0.));
#5471=DIRECTION('ref_axis',(1.,0.,0.));
#5472=DIRECTION('',(-0.447213595499958,0.894427190999916,-5.47678698264203E-17));
#5473=DIRECTION('center_axis',(0.,-1.,0.));
#5474=DIRECTION('ref_axis',(1.,0.,0.));
#5475=DIRECTION('center_axis',(0.,1.,0.));
#5476=DIRECTION('ref_axis',(1.,0.,0.));
#5477=DIRECTION('',(0.,1.,0.));
#5478=DIRECTION('center_axis',(0.,1.,0.));
#5479=DIRECTION('ref_axis',(1.,0.,0.));
#5480=DIRECTION('center_axis',(0.,-1.,0.));
#5481=DIRECTION('ref_axis',(1.,0.,0.));
#5482=DIRECTION('',(-0.707106781186547,0.707106781186548,-8.65956056235493E-17));
#5483=DIRECTION('center_axis',(0.,-1.,0.));
#5484=DIRECTION('ref_axis',(0.,0.,-1.));
#5485=DIRECTION('center_axis',(0.866025403784439,0.,-0.5));
#5486=DIRECTION('ref_axis',(0.5,0.,0.866025403784439));
#5487=DIRECTION('',(-0.5,0.,-0.866025403784439));
#5488=DIRECTION('',(0.,-1.,0.));
#5489=DIRECTION('',(0.5,0.,0.866025403784439));
#5490=DIRECTION('',(0.,-1.,0.));
#5491=DIRECTION('center_axis',(1.20185167898973E-16,0.,-1.));
#5492=DIRECTION('ref_axis',(1.,0.,1.20185167898973E-16));
#5493=DIRECTION('',(-1.,0.,-1.20185167898973E-16));
#5494=DIRECTION('',(0.,-1.,0.));
#5495=DIRECTION('',(1.,0.,1.20185167898973E-16));
#5496=DIRECTION('center_axis',(-0.866025403784439,0.,-0.5));
#5497=DIRECTION('ref_axis',(0.5,0.,-0.866025403784439));
#5498=DIRECTION('',(-0.5,0.,0.866025403784439));
#5499=DIRECTION('',(0.,-1.,0.));
#5500=DIRECTION('',(0.5,0.,-0.866025403784439));
#5501=DIRECTION('center_axis',(-0.866025403784439,0.,0.5));
#5502=DIRECTION('ref_axis',(-0.5,0.,-0.866025403784439));
#5503=DIRECTION('',(0.5,0.,0.866025403784439));
#5504=DIRECTION('',(0.,-1.,0.));
#5505=DIRECTION('',(-0.5,0.,-0.866025403784439));
#5506=DIRECTION('center_axis',(-2.40370335797945E-16,0.,1.));
#5507=DIRECTION('ref_axis',(-1.,0.,-2.40370335797945E-16));
#5508=DIRECTION('',(1.,0.,2.40370335797945E-16));
#5509=DIRECTION('',(0.,-1.,0.));
#5510=DIRECTION('',(-1.,0.,-2.40370335797945E-16));
#5511=DIRECTION('center_axis',(0.866025403784439,0.,0.5));
#5512=DIRECTION('ref_axis',(-0.5,0.,0.866025403784439));
#5513=DIRECTION('',(0.5,0.,-0.866025403784439));
#5514=DIRECTION('',(-0.5,0.,0.866025403784439));
#5515=DIRECTION('center_axis',(0.,1.,0.));
#5516=DIRECTION('ref_axis',(1.,0.,0.));
#5517=DIRECTION('center_axis',(0.,-1.,0.));
#5518=DIRECTION('ref_axis',(0.,0.,-1.));
#5519=DIRECTION('axis',(0.,0.,1.));
#5520=DIRECTION('refdir',(1.,0.,0.));
#5521=DIRECTION('axis',(0.,0.,1.));
#5522=DIRECTION('refdir',(1.,0.,0.));
#5523=DIRECTION('center_axis',(0.,1.,0.));
#5524=DIRECTION('ref_axis',(0.,0.,1.));
#5525=DIRECTION('center_axis',(0.,-1.,0.));
#5526=DIRECTION('ref_axis',(1.,0.,0.));
#5527=DIRECTION('',(-1.,0.,0.));
#5528=DIRECTION('',(0.,0.,-1.));
#5529=DIRECTION('',(1.,0.,0.));
#5530=DIRECTION('center_axis',(0.,0.,1.));
#5531=DIRECTION('ref_axis',(1.,0.,0.));
#5532=DIRECTION('',(0.,-1.,0.));
#5533=DIRECTION('',(0.,1.,0.));
#5534=DIRECTION('',(-1.,0.,0.));
#5535=DIRECTION('center_axis',(0.,-1.,0.));
#5536=DIRECTION('ref_axis',(0.,0.,-1.));
#5537=DIRECTION('center_axis',(0.,1.,0.));
#5538=DIRECTION('ref_axis',(1.,0.,0.));
#5539=DIRECTION('',(0.,0.,1.));
#5540=DIRECTION('',(1.,0.,0.));
#5541=DIRECTION('center_axis',(0.,0.,-1.));
#5542=DIRECTION('ref_axis',(-1.,0.,0.));
#5543=DIRECTION('',(0.,1.,0.));
#5544=DIRECTION('',(0.,1.,0.));
#5545=DIRECTION('center_axis',(1.,0.,0.));
#5546=DIRECTION('ref_axis',(0.,0.,-1.));
#5547=DIRECTION('center_axis',(0.,1.,0.));
#5548=DIRECTION('ref_axis',(0.,0.,1.));
#5549=DIRECTION('center_axis',(0.,-1.,0.));
#5550=DIRECTION('ref_axis',(1.,0.,0.));
#5551=DIRECTION('center_axis',(0.,-1.,0.));
#5552=DIRECTION('ref_axis',(1.,0.,0.));
#5553=DIRECTION('center_axis',(0.,-1.,0.));
#5554=DIRECTION('ref_axis',(1.,0.,0.));
#5555=DIRECTION('center_axis',(0.,-1.,0.));
#5556=DIRECTION('ref_axis',(1.,0.,0.));
#5557=DIRECTION('',(0.,1.,0.));
#5558=DIRECTION('center_axis',(0.,-1.,0.));
#5559=DIRECTION('ref_axis',(0.,0.,-1.));
#5560=DIRECTION('center_axis',(0.,-1.,0.));
#5561=DIRECTION('ref_axis',(1.,0.,0.));
#5562=DIRECTION('center_axis',(0.,-1.,0.));
#5563=DIRECTION('ref_axis',(1.,0.,0.));
#5564=DIRECTION('center_axis',(0.,-1.,0.));
#5565=DIRECTION('ref_axis',(1.,0.,0.));
#5566=DIRECTION('',(0.,1.,0.));
#5567=DIRECTION('center_axis',(0.,1.,0.));
#5568=DIRECTION('ref_axis',(0.,0.,1.));
#5569=DIRECTION('center_axis',(0.,-1.,0.));
#5570=DIRECTION('ref_axis',(1.,0.,0.));
#5571=DIRECTION('center_axis',(0.,-1.,0.));
#5572=DIRECTION('ref_axis',(1.,0.,0.));
#5573=DIRECTION('center_axis',(0.,-1.,0.));
#5574=DIRECTION('ref_axis',(1.,0.,0.));
#5575=DIRECTION('',(0.,1.,0.));
#5576=DIRECTION('center_axis',(0.,-1.,0.));
#5577=DIRECTION('ref_axis',(0.,0.,-1.));
#5578=DIRECTION('center_axis',(0.,-1.,0.));
#5579=DIRECTION('ref_axis',(1.,0.,0.));
#5580=DIRECTION('center_axis',(0.,-1.,0.));
#5581=DIRECTION('ref_axis',(1.,0.,0.));
#5582=DIRECTION('center_axis',(0.,-1.,0.));
#5583=DIRECTION('ref_axis',(1.,0.,0.));
#5584=DIRECTION('',(0.,1.,0.));
#5585=DIRECTION('center_axis',(0.,1.,0.));
#5586=DIRECTION('ref_axis',(0.,0.,1.));
#5587=DIRECTION('center_axis',(0.,-1.,0.));
#5588=DIRECTION('ref_axis',(1.,0.,0.));
#5589=DIRECTION('center_axis',(0.,-1.,0.));
#5590=DIRECTION('ref_axis',(1.,0.,0.));
#5591=DIRECTION('center_axis',(0.,-1.,0.));
#5592=DIRECTION('ref_axis',(1.,0.,0.));
#5593=DIRECTION('',(0.,1.,0.));
#5594=DIRECTION('center_axis',(0.,-1.,0.));
#5595=DIRECTION('ref_axis',(0.,0.,-1.));
#5596=DIRECTION('center_axis',(0.,-1.,0.));
#5597=DIRECTION('ref_axis',(1.,0.,0.));
#5598=DIRECTION('center_axis',(0.,-1.,0.));
#5599=DIRECTION('ref_axis',(1.,0.,0.));
#5600=DIRECTION('',(0.,1.,0.));
#5601=DIRECTION('axis',(0.,0.,1.));
#5602=DIRECTION('refdir',(1.,0.,0.));
#5603=DIRECTION('center_axis',(0.,1.,0.));
#5604=DIRECTION('ref_axis',(0.,0.,1.));
#5605=DIRECTION('center_axis',(0.,1.,0.));
#5606=DIRECTION('ref_axis',(1.,0.,0.));
#5607=DIRECTION('',(1.,0.,0.));
#5608=DIRECTION('center_axis',(0.,-1.,0.));
#5609=DIRECTION('ref_axis',(1.,0.,0.));
#5610=DIRECTION('',(-1.,0.,0.));
#5611=DIRECTION('center_axis',(0.,0.,-1.));
#5612=DIRECTION('ref_axis',(-1.,0.,0.));
#5613=DIRECTION('',(0.,-1.,0.));
#5614=DIRECTION('',(0.,1.,0.));
#5615=DIRECTION('',(1.,0.,0.));
#5616=DIRECTION('center_axis',(0.,-1.,0.));
#5617=DIRECTION('ref_axis',(0.,0.,-1.));
#5618=DIRECTION('center_axis',(0.,-1.,0.));
#5619=DIRECTION('ref_axis',(1.,0.,0.));
#5620=DIRECTION('center_axis',(0.,1.,0.));
#5621=DIRECTION('ref_axis',(1.,0.,0.));
#5622=DIRECTION('',(-1.,0.,0.));
#5623=DIRECTION('center_axis',(0.,0.,1.));
#5624=DIRECTION('ref_axis',(1.,0.,0.));
#5625=DIRECTION('',(0.,1.,0.));
#5626=DIRECTION('',(0.,-1.,0.));
#5627=DIRECTION('center_axis',(0.,1.,0.));
#5628=DIRECTION('ref_axis',(0.,0.,1.));
#5629=DIRECTION('center_axis',(0.,-1.,0.));
#5630=DIRECTION('ref_axis',(1.,0.,0.));
#5631=DIRECTION('center_axis',(0.,-1.,0.));
#5632=DIRECTION('ref_axis',(1.,0.,0.));
#5633=DIRECTION('center_axis',(0.,-1.,0.));
#5634=DIRECTION('ref_axis',(1.,0.,0.));
#5635=DIRECTION('center_axis',(0.,-1.,0.));
#5636=DIRECTION('ref_axis',(1.,0.,0.));
#5637=DIRECTION('',(0.,1.,0.));
#5638=DIRECTION('center_axis',(0.,-1.,0.));
#5639=DIRECTION('ref_axis',(0.,0.,-1.));
#5640=DIRECTION('center_axis',(0.,-1.,0.));
#5641=DIRECTION('ref_axis',(1.,0.,0.));
#5642=DIRECTION('center_axis',(0.,-1.,0.));
#5643=DIRECTION('ref_axis',(1.,0.,0.));
#5644=DIRECTION('',(0.,1.,0.));
#5645=DIRECTION('',(0.,0.,1.));
#5646=DIRECTION('',(1.,0.,0.));
#5647=DIRECTION('',(0.,0.,1.));
#5648=DIRECTION('',(1.,0.,0.));
#5649=DIRECTION('axis',(0.,0.,1.));
#5650=DIRECTION('refdir',(1.,0.,0.));
#5651=DIRECTION('axis',(0.,0.,1.));
#5652=DIRECTION('refdir',(1.,0.,0.));
#5653=DIRECTION('center_axis',(0.,0.,1.));
#5654=DIRECTION('ref_axis',(1.,0.,0.));
#5655=DIRECTION('',(1.,0.,0.));
#5656=DIRECTION('center_axis',(0.,0.,1.));
#5657=DIRECTION('ref_axis',(1.,0.,0.));
#5658=DIRECTION('center_axis',(0.,0.,1.));
#5659=DIRECTION('ref_axis',(1.,0.,0.));
#5660=DIRECTION('center_axis',(0.,0.,1.));
#5661=DIRECTION('ref_axis',(1.,0.,0.));
#5662=DIRECTION('',(0.,0.,1.));
#5663=DIRECTION('center_axis',(0.,0.,1.));
#5664=DIRECTION('ref_axis',(1.,0.,0.));
#5665=DIRECTION('',(-1.,0.,0.));
#5666=DIRECTION('center_axis',(1.,0.,0.));
#5667=DIRECTION('ref_axis',(0.,0.,-1.));
#5668=DIRECTION('center_axis',(-1.,0.,0.));
#5669=DIRECTION('ref_axis',(0.,0.,-1.));
#5670=DIRECTION('',(-1.,0.,0.));
#5671=DIRECTION('',(-1.,0.,0.));
#5672=DIRECTION('center_axis',(-1.,0.,0.));
#5673=DIRECTION('ref_axis',(0.,0.,-1.));
#5674=DIRECTION('center_axis',(1.,0.,0.));
#5675=DIRECTION('ref_axis',(0.,0.,-1.));
#5676=DIRECTION('center_axis',(1.,0.,0.));
#5677=DIRECTION('ref_axis',(0.,0.,-1.));
#5678=DIRECTION('',(-1.,0.,0.));
#5679=DIRECTION('',(-1.,0.,0.));
#5680=DIRECTION('center_axis',(1.,0.,0.));
#5681=DIRECTION('ref_axis',(0.,0.,-1.));
#5682=DIRECTION('center_axis',(1.,0.,0.));
#5683=DIRECTION('ref_axis',(0.,0.,-1.));
#5684=DIRECTION('center_axis',(1.,0.,0.));
#5685=DIRECTION('ref_axis',(0.,0.,-1.));
#5686=DIRECTION('axis',(0.,0.,1.));
#5687=DIRECTION('refdir',(1.,0.,0.));
#5688=DIRECTION('center_axis',(0.,0.,1.));
#5689=DIRECTION('ref_axis',(1.,0.,0.));
#5690=DIRECTION('',(1.,0.,0.));
#5691=DIRECTION('center_axis',(0.,0.,1.));
#5692=DIRECTION('ref_axis',(1.,0.,0.));
#5693=DIRECTION('center_axis',(0.,0.,1.));
#5694=DIRECTION('ref_axis',(1.,0.,0.));
#5695=DIRECTION('center_axis',(0.,0.,1.));
#5696=DIRECTION('ref_axis',(1.,0.,0.));
#5697=DIRECTION('',(0.,0.,1.));
#5698=DIRECTION('center_axis',(0.,0.,1.));
#5699=DIRECTION('ref_axis',(1.,0.,0.));
#5700=DIRECTION('',(-1.,0.,0.));
#5701=DIRECTION('center_axis',(1.,0.,0.));
#5702=DIRECTION('ref_axis',(0.,0.,-1.));
#5703=DIRECTION('center_axis',(-1.,0.,0.));
#5704=DIRECTION('ref_axis',(0.,0.,-1.));
#5705=DIRECTION('',(-1.,0.,0.));
#5706=DIRECTION('',(-1.,0.,0.));
#5707=DIRECTION('center_axis',(-1.,0.,0.));
#5708=DIRECTION('ref_axis',(0.,0.,-1.));
#5709=DIRECTION('center_axis',(1.,0.,0.));
#5710=DIRECTION('ref_axis',(0.,0.,-1.));
#5711=DIRECTION('center_axis',(1.,0.,0.));
#5712=DIRECTION('ref_axis',(0.,0.,-1.));
#5713=DIRECTION('',(-1.,0.,0.));
#5714=DIRECTION('',(-1.,0.,0.));
#5715=DIRECTION('center_axis',(1.,0.,0.));
#5716=DIRECTION('ref_axis',(0.,0.,-1.));
#5717=DIRECTION('center_axis',(1.,0.,0.));
#5718=DIRECTION('ref_axis',(0.,0.,-1.));
#5719=DIRECTION('center_axis',(1.,0.,0.));
#5720=DIRECTION('ref_axis',(0.,0.,-1.));
#5721=DIRECTION('axis',(0.,0.,1.));
#5722=DIRECTION('refdir',(1.,0.,0.));
#5723=DIRECTION('center_axis',(1.,0.,0.));
#5724=DIRECTION('ref_axis',(0.,0.,-1.));
#5725=DIRECTION('center_axis',(1.,0.,0.));
#5726=DIRECTION('ref_axis',(0.,0.,-1.));
#5727=DIRECTION('',(1.,0.,0.));
#5728=DIRECTION('center_axis',(-1.,0.,0.));
#5729=DIRECTION('ref_axis',(0.,0.,-1.));
#5730=DIRECTION('center_axis',(1.,0.,0.));
#5731=DIRECTION('ref_axis',(0.,0.,-1.));
#5732=DIRECTION('center_axis',(1.,0.,0.));
#5733=DIRECTION('ref_axis',(0.,0.,-1.));
#5734=DIRECTION('center_axis',(1.,0.,0.));
#5735=DIRECTION('ref_axis',(0.,0.,-1.));
#5736=DIRECTION('',(-1.,0.,0.));
#5737=DIRECTION('center_axis',(-1.,0.,0.));
#5738=DIRECTION('ref_axis',(0.,0.,-1.));
#5739=DIRECTION('center_axis',(1.,0.,0.));
#5740=DIRECTION('ref_axis',(0.,0.,-1.));
#5741=DIRECTION('center_axis',(1.,0.,0.));
#5742=DIRECTION('ref_axis',(0.,0.,-1.));
#5743=DIRECTION('',(-1.,0.,0.));
#5744=DIRECTION('center_axis',(1.,0.,0.));
#5745=DIRECTION('ref_axis',(0.,0.,-1.));
#5746=DIRECTION('center_axis',(1.,0.,0.));
#5747=DIRECTION('ref_axis',(0.,0.,-1.));
#5748=DIRECTION('center_axis',(1.,0.,0.));
#5749=DIRECTION('ref_axis',(0.,0.,-1.));
#5750=DIRECTION('axis',(0.,0.,1.));
#5751=DIRECTION('refdir',(1.,0.,0.));
#5752=DIRECTION('center_axis',(1.,0.,0.));
#5753=DIRECTION('ref_axis',(0.,0.,-1.));
#5754=DIRECTION('center_axis',(1.,0.,0.));
#5755=DIRECTION('ref_axis',(0.,0.,-1.));
#5756=DIRECTION('',(1.,0.,0.));
#5757=DIRECTION('center_axis',(-1.,0.,0.));
#5758=DIRECTION('ref_axis',(0.,0.,-1.));
#5759=DIRECTION('center_axis',(1.,0.,0.));
#5760=DIRECTION('ref_axis',(0.,0.,-1.));
#5761=DIRECTION('center_axis',(1.,0.,0.));
#5762=DIRECTION('ref_axis',(0.,0.,-1.));
#5763=DIRECTION('center_axis',(-1.,0.,0.));
#5764=DIRECTION('ref_axis',(0.,0.,-1.));
#5765=DIRECTION('',(-0.707106781186548,8.65956056235493E-17,-0.707106781186547));
#5766=DIRECTION('center_axis',(1.,0.,0.));
#5767=DIRECTION('ref_axis',(0.,0.,-1.));
#5768=DIRECTION('center_axis',(1.,0.,0.));
#5769=DIRECTION('ref_axis',(0.,0.,-1.));
#5770=DIRECTION('center_axis',(1.,0.,0.));
#5771=DIRECTION('ref_axis',(0.,0.,-1.));
#5772=DIRECTION('',(-1.,0.,0.));
#5773=DIRECTION('center_axis',(1.,0.,0.));
#5774=DIRECTION('ref_axis',(0.,0.,-1.));
#5775=DIRECTION('center_axis',(-1.,0.,0.));
#5776=DIRECTION('ref_axis',(0.,0.,-1.));
#5777=DIRECTION('center_axis',(-1.,0.,0.));
#5778=DIRECTION('ref_axis',(0.,0.,-1.));
#5779=DIRECTION('',(-0.707106781186553,-8.65956056235487E-17,0.707106781186542));
#5780=DIRECTION('center_axis',(1.,0.,0.));
#5781=DIRECTION('ref_axis',(0.,0.,-1.));
#5782=DIRECTION('axis',(0.,0.,1.));
#5783=DIRECTION('refdir',(1.,0.,0.));
#5784=DIRECTION('center_axis',(0.866025403784439,0.,-0.5));
#5785=DIRECTION('ref_axis',(0.5,0.,0.866025403784439));
#5786=DIRECTION('',(0.5,0.,0.866025403784439));
#5787=DIRECTION('',(0.,-1.,0.));
#5788=DIRECTION('',(0.5,0.,0.866025403784439));
#5789=DIRECTION('',(0.,-1.,0.));
#5790=DIRECTION('center_axis',(1.92296268638356E-16,0.,-1.));
#5791=DIRECTION('ref_axis',(1.,0.,1.92296268638356E-16));
#5792=DIRECTION('',(1.,0.,1.92296268638356E-16));
#5793=DIRECTION('',(0.,-1.,0.));
#5794=DIRECTION('',(1.,0.,1.92296268638356E-16));
#5795=DIRECTION('center_axis',(-0.866025403784439,0.,-0.5));
#5796=DIRECTION('ref_axis',(0.5,0.,-0.866025403784439));
#5797=DIRECTION('',(0.5,0.,-0.866025403784439));
#5798=DIRECTION('',(0.,-1.,0.));
#5799=DIRECTION('',(0.5,0.,-0.866025403784438));
#5800=DIRECTION('center_axis',(-0.866025403784439,0.,0.5));
#5801=DIRECTION('ref_axis',(-0.5,0.,-0.866025403784439));
#5802=DIRECTION('',(-0.5,0.,-0.866025403784439));
#5803=DIRECTION('',(0.,-1.,0.));
#5804=DIRECTION('',(-0.5,0.,-0.866025403784439));
#5805=DIRECTION('center_axis',(-1.92296268638356E-16,0.,1.));
#5806=DIRECTION('ref_axis',(-1.,0.,-1.92296268638356E-16));
#5807=DIRECTION('',(-1.,0.,-1.92296268638356E-16));
#5808=DIRECTION('',(0.,-1.,0.));
#5809=DIRECTION('',(-1.,0.,-1.92296268638356E-16));
#5810=DIRECTION('center_axis',(0.866025403784439,0.,0.5));
#5811=DIRECTION('ref_axis',(-0.5,0.,0.866025403784439));
#5812=DIRECTION('',(-0.5,0.,0.866025403784439));
#5813=DIRECTION('',(-0.5,0.,0.866025403784439));
#5814=DIRECTION('center_axis',(0.,-1.,0.));
#5815=DIRECTION('ref_axis',(0.,0.,-1.));
#5816=DIRECTION('center_axis',(0.,1.,0.));
#5817=DIRECTION('ref_axis',(0.,0.,1.));
#5818=DIRECTION('center_axis',(0.,-1.,0.));
#5819=DIRECTION('ref_axis',(1.,0.,0.));
#5820=DIRECTION('center_axis',(0.,-1.,0.));
#5821=DIRECTION('ref_axis',(1.,0.,0.));
#5822=DIRECTION('center_axis',(0.,-1.,0.));
#5823=DIRECTION('ref_axis',(1.,0.,0.));
#5824=DIRECTION('',(0.707106781186547,0.707106781186548,8.65956056235493E-17));
#5825=DIRECTION('center_axis',(0.,-1.,0.));
#5826=DIRECTION('ref_axis',(1.,0.,0.));
#5827=DIRECTION('center_axis',(0.,1.,0.));
#5828=DIRECTION('ref_axis',(1.,0.,0.));
#5829=DIRECTION('',(0.,1.,0.));
#5830=DIRECTION('center_axis',(0.,1.,0.));
#5831=DIRECTION('ref_axis',(1.,0.,0.));
#5832=DIRECTION('center_axis',(0.,-1.,0.));
#5833=DIRECTION('ref_axis',(1.,0.,0.));
#5834=DIRECTION('',(-0.707106781186547,0.707106781186548,-8.65956056235493E-17));
#5835=DIRECTION('center_axis',(0.,-1.,0.));
#5836=DIRECTION('ref_axis',(0.,0.,-1.));
#5837=DIRECTION('axis',(0.,0.,1.));
#5838=DIRECTION('refdir',(1.,0.,0.));
#5839=DIRECTION('center_axis',(0.,1.,0.));
#5840=DIRECTION('ref_axis',(0.,0.,1.));
#5841=DIRECTION('center_axis',(0.,-1.,0.));
#5842=DIRECTION('ref_axis',(1.,0.,0.));
#5843=DIRECTION('center_axis',(0.,-1.,0.));
#5844=DIRECTION('ref_axis',(1.,0.,0.));
#5845=DIRECTION('center_axis',(0.,-1.,0.));
#5846=DIRECTION('ref_axis',(1.,0.,0.));
#5847=DIRECTION('',(0.707106781186547,0.707106781186548,8.65956056235493E-17));
#5848=DIRECTION('center_axis',(0.,-1.,0.));
#5849=DIRECTION('ref_axis',(1.,0.,0.));
#5850=DIRECTION('center_axis',(0.,-1.,0.));
#5851=DIRECTION('ref_axis',(1.,0.,0.));
#5852=DIRECTION('',(0.,1.,0.));
#5853=DIRECTION('center_axis',(0.,1.,0.));
#5854=DIRECTION('ref_axis',(1.,0.,0.));
#5855=DIRECTION('center_axis',(0.,-1.,0.));
#5856=DIRECTION('ref_axis',(1.,0.,0.));
#5857=DIRECTION('',(-0.707106781186547,0.707106781186548,-8.65956056235493E-17));
#5858=DIRECTION('center_axis',(0.,-1.,0.));
#5859=DIRECTION('ref_axis',(0.,0.,-1.));
#5860=DIRECTION('center_axis',(0.,-1.,0.));
#5861=DIRECTION('ref_axis',(1.,0.,0.));
#5862=DIRECTION('center_axis',(0.,1.,0.));
#5863=DIRECTION('ref_axis',(1.,0.,0.));
#5864=DIRECTION('center_axis',(0.,1.,0.));
#5865=DIRECTION('ref_axis',(1.,0.,0.));
#5866=DIRECTION('',(-0.447213595499958,0.894427190999916,-5.47678698264203E-17));
#5867=DIRECTION('center_axis',(0.,-1.,0.));
#5868=DIRECTION('ref_axis',(1.,0.,0.));
#5869=DIRECTION('center_axis',(0.,1.,0.));
#5870=DIRECTION('ref_axis',(1.,0.,0.));
#5871=DIRECTION('',(0.,1.,0.));
#5872=DIRECTION('center_axis',(0.,1.,0.));
#5873=DIRECTION('ref_axis',(1.,0.,0.));
#5874=DIRECTION('center_axis',(0.,-1.,0.));
#5875=DIRECTION('ref_axis',(1.,0.,0.));
#5876=DIRECTION('',(-0.707106781186547,0.707106781186548,-8.65956056235493E-17));
#5877=DIRECTION('center_axis',(0.,-1.,0.));
#5878=DIRECTION('ref_axis',(0.,0.,-1.));
#5879=DIRECTION('center_axis',(0.866025403784439,0.,-0.5));
#5880=DIRECTION('ref_axis',(0.5,0.,0.866025403784439));
#5881=DIRECTION('',(-0.5,0.,-0.866025403784439));
#5882=DIRECTION('',(0.,-1.,0.));
#5883=DIRECTION('',(0.5,0.,0.866025403784439));
#5884=DIRECTION('',(0.,-1.,0.));
#5885=DIRECTION('center_axis',(1.60246890531964E-16,0.,-1.));
#5886=DIRECTION('ref_axis',(1.,0.,1.60246890531964E-16));
#5887=DIRECTION('',(-1.,0.,-1.60246890531964E-16));
#5888=DIRECTION('',(0.,-1.,0.));
#5889=DIRECTION('',(1.,0.,1.60246890531964E-16));
#5890=DIRECTION('center_axis',(-0.866025403784439,0.,-0.5));
#5891=DIRECTION('ref_axis',(0.5,0.,-0.866025403784439));
#5892=DIRECTION('',(-0.5,0.,0.866025403784439));
#5893=DIRECTION('',(0.,-1.,0.));
#5894=DIRECTION('',(0.5,0.,-0.866025403784439));
#5895=DIRECTION('center_axis',(-0.866025403784439,0.,0.5));
#5896=DIRECTION('ref_axis',(-0.5,0.,-0.866025403784439));
#5897=DIRECTION('',(0.5,0.,0.866025403784439));
#5898=DIRECTION('',(0.,-1.,0.));
#5899=DIRECTION('',(-0.5,0.,-0.866025403784439));
#5900=DIRECTION('center_axis',(-1.60246890531964E-16,0.,1.));
#5901=DIRECTION('ref_axis',(-1.,0.,-1.60246890531964E-16));
#5902=DIRECTION('',(1.,0.,1.60246890531964E-16));
#5903=DIRECTION('',(0.,-1.,0.));
#5904=DIRECTION('',(-1.,0.,-1.60246890531964E-16));
#5905=DIRECTION('center_axis',(0.866025403784439,0.,0.5));
#5906=DIRECTION('ref_axis',(-0.5,0.,0.866025403784439));
#5907=DIRECTION('',(0.5,0.,-0.866025403784439));
#5908=DIRECTION('',(-0.5,0.,0.866025403784439));
#5909=DIRECTION('center_axis',(0.,1.,0.));
#5910=DIRECTION('ref_axis',(1.,0.,0.));
#5911=DIRECTION('center_axis',(0.,-1.,0.));
#5912=DIRECTION('ref_axis',(0.,0.,-1.));
#5913=DIRECTION('',(0.,0.,1.));
#5914=DIRECTION('',(1.,0.,0.));
#5915=DIRECTION('',(0.,0.,1.));
#5916=DIRECTION('',(1.,0.,0.));
#5917=DIRECTION('',(0.,0.,1.));
#5918=DIRECTION('',(1.,0.,0.));
#5919=DIRECTION('',(0.,0.,1.));
#5920=DIRECTION('',(1.,0.,0.));
#5921=DIRECTION('',(0.,0.,1.));
#5922=DIRECTION('',(1.,0.,0.));
#5923=DIRECTION('',(0.,0.,1.));
#5924=DIRECTION('',(1.,0.,0.));
#5925=DIRECTION('',(0.,0.,1.));
#5926=DIRECTION('',(1.,0.,0.));
#5927=DIRECTION('',(0.,0.,1.));
#5928=DIRECTION('',(1.,0.,0.));
#5929=DIRECTION('',(0.,0.,1.));
#5930=DIRECTION('',(1.,0.,0.));
#5931=DIRECTION('',(0.,0.,1.));
#5932=DIRECTION('',(1.,0.,0.));
#5933=DIRECTION('',(0.,0.,1.));
#5934=DIRECTION('',(1.,0.,0.));
#5935=DIRECTION('',(0.,1.,2.22044604925031E-16));
#5936=DIRECTION('',(1.,0.,0.));
#5937=DIRECTION('',(0.,-1.,2.22044604925031E-16));
#5938=DIRECTION('',(1.,0.,0.));
#5939=DIRECTION('',(0.,1.,2.22044604925031E-16));
#5940=DIRECTION('',(1.,0.,0.));
#5941=DIRECTION('',(0.,-1.,2.22044604925031E-16));
#5942=DIRECTION('',(1.,0.,0.));
#5943=DIRECTION('',(0.,1.,2.22044604925031E-16));
#5944=DIRECTION('',(1.,0.,0.));
#5945=DIRECTION('',(0.,-1.,2.22044604925031E-16));
#5946=DIRECTION('',(1.,0.,0.));
#5947=DIRECTION('',(0.,1.,2.22044604925031E-16));
#5948=DIRECTION('',(1.,0.,0.));
#5949=DIRECTION('',(0.,-1.,2.22044604925031E-16));
#5950=DIRECTION('',(1.,0.,0.));
#5951=DIRECTION('',(0.,0.,1.));
#5952=DIRECTION('',(2.22044604925031E-16,-1.,0.));
#5953=DIRECTION('',(0.,0.,1.));
#5954=DIRECTION('',(2.22044604925031E-16,-1.,0.));
#5955=DIRECTION('',(0.,0.,1.));
#5956=DIRECTION('',(2.22044604925031E-16,1.,0.));
#5957=DIRECTION('',(0.,0.,1.));
#5958=DIRECTION('',(2.22044604925031E-16,1.,0.));
#5959=DIRECTION('',(0.,0.,1.));
#5960=DIRECTION('',(2.22044604925031E-16,1.,0.));
#5961=DIRECTION('',(0.,-1.,2.22044604925031E-16));
#5962=DIRECTION('',(1.,0.,0.));
#5963=DIRECTION('',(0.,0.,1.));
#5964=DIRECTION('',(2.22044604925031E-16,-1.,0.));
#5965=DIRECTION('',(0.,0.,1.));
#5966=DIRECTION('',(2.22044604925031E-16,-1.,0.));
#5967=DIRECTION('',(0.,0.,1.));
#5968=DIRECTION('',(2.22044604925031E-16,-1.,0.));
#5969=DIRECTION('',(0.,0.,1.));
#5970=DIRECTION('',(1.,0.,0.));
#5971=DIRECTION('',(0.,0.,1.));
#5972=DIRECTION('',(1.,0.,0.));
#5973=DIRECTION('',(0.,0.,1.));
#5974=DIRECTION('',(1.,0.,0.));
#5975=DIRECTION('',(0.,0.,1.));
#5976=DIRECTION('',(1.,0.,0.));
#5977=DIRECTION('',(0.,-1.,2.22044604925031E-16));
#5978=DIRECTION('',(1.,0.,0.));
#5979=DIRECTION('',(0.,-1.,2.22044604925031E-16));
#5980=DIRECTION('',(1.,0.,0.));
#5981=DIRECTION('',(0.,0.,1.));
#5982=DIRECTION('',(2.22044604925031E-16,-1.,0.));
#5983=DIRECTION('',(0.,0.,1.));
#5984=DIRECTION('',(1.,0.,0.));
#5985=DIRECTION('',(0.,0.,1.));
#5986=DIRECTION('',(1.,0.,0.));
#5987=CARTESIAN_POINT('',(0.,0.,0.));
#5988=CARTESIAN_POINT('',(0.,0.,0.));
#5989=CARTESIAN_POINT('',(0.,0.,0.));
#5990=CARTESIAN_POINT('Origin',(7.8,-2.1,-0.1));
#5991=CARTESIAN_POINT('',(7.525,-2.1,0.));
#5992=CARTESIAN_POINT('Origin',(7.8,-2.1,0.));
#5993=CARTESIAN_POINT('',(7.525,-2.1,1.));
#5994=CARTESIAN_POINT('',(7.525,-2.1,-0.1));
#5995=CARTESIAN_POINT('Origin',(7.8,-2.1,1.));
#5996=CARTESIAN_POINT('Origin',(2.2,2.1,-0.1));
#5997=CARTESIAN_POINT('',(1.925,2.1,0.));
#5998=CARTESIAN_POINT('Origin',(2.2,2.1,0.));
#5999=CARTESIAN_POINT('',(1.925,2.1,1.));
#6000=CARTESIAN_POINT('',(1.925,2.1,-0.1));
#6001=CARTESIAN_POINT('Origin',(2.2,2.1,1.));
#6002=CARTESIAN_POINT('Origin',(2.2,-2.1,-0.1));
#6003=CARTESIAN_POINT('',(1.925,-2.1,0.));
#6004=CARTESIAN_POINT('Origin',(2.2,-2.1,0.));
#6005=CARTESIAN_POINT('',(1.925,-2.1,1.));
#6006=CARTESIAN_POINT('',(1.925,-2.1,-0.1));
#6007=CARTESIAN_POINT('Origin',(2.2,-2.1,1.));
#6008=CARTESIAN_POINT('Origin',(7.8,2.1,-0.1));
#6009=CARTESIAN_POINT('',(7.525,2.1,0.));
#6010=CARTESIAN_POINT('Origin',(7.8,2.1,0.));
#6011=CARTESIAN_POINT('',(7.525,2.1,1.));
#6012=CARTESIAN_POINT('',(7.525,2.1,-0.1));
#6013=CARTESIAN_POINT('Origin',(7.8,2.1,1.));
#6014=CARTESIAN_POINT('Origin',(14.,3.5,0.));
#6015=CARTESIAN_POINT('',(14.,3.5,0.));
#6016=CARTESIAN_POINT('',(-2.,3.5,0.));
#6017=CARTESIAN_POINT('',(14.,3.5,0.));
#6018=CARTESIAN_POINT('',(-2.,3.5,1.));
#6019=CARTESIAN_POINT('',(-2.,3.5,0.));
#6020=CARTESIAN_POINT('',(14.,3.5,1.));
#6021=CARTESIAN_POINT('',(14.,3.5,1.));
#6022=CARTESIAN_POINT('',(14.,3.5,0.));
#6023=CARTESIAN_POINT('Origin',(14.,-3.5,0.));
#6024=CARTESIAN_POINT('',(14.,-3.5,0.));
#6025=CARTESIAN_POINT('',(14.,-3.5,0.));
#6026=CARTESIAN_POINT('',(14.,-3.5,1.));
#6027=CARTESIAN_POINT('',(14.,-3.5,1.));
#6028=CARTESIAN_POINT('',(14.,-3.5,0.));
#6029=CARTESIAN_POINT('Origin',(-2.,-3.5,0.));
#6030=CARTESIAN_POINT('',(-2.,-3.5,0.));
#6031=CARTESIAN_POINT('',(-2.,-3.5,0.));
#6032=CARTESIAN_POINT('',(-2.,-3.5,1.));
#6033=CARTESIAN_POINT('',(-2.,-3.5,1.));
#6034=CARTESIAN_POINT('',(-2.,-3.5,0.));
#6035=CARTESIAN_POINT('Origin',(-2.,3.5,0.));
#6036=CARTESIAN_POINT('',(-2.,3.5,0.));
#6037=CARTESIAN_POINT('',(-2.,3.5,1.));
#6038=CARTESIAN_POINT('Origin',(6.,0.,1.));
#6039=CARTESIAN_POINT('Origin',(6.,0.,0.));
#6040=CARTESIAN_POINT('',(0.,0.,0.));
#6041=CARTESIAN_POINT('Origin',(8.4,1.04094977927525E-16,5.2));
#6042=CARTESIAN_POINT('',(8.4,0.12722459888658,5.09493382352941));
#6043=CARTESIAN_POINT('',(9.,0.127224598886581,5.09493382352941));
#6044=CARTESIAN_POINT('',(8.4,0.12722459888658,5.09493382352941));
#6045=CARTESIAN_POINT('',(8.4,-0.12722459888658,5.09493382352941));
#6046=CARTESIAN_POINT('Origin',(8.4,1.04094977927525E-16,5.2));
#6047=CARTESIAN_POINT('',(9.,-0.127224598886581,5.09493382352941));
#6048=CARTESIAN_POINT('',(8.4,-0.12722459888658,5.09493382352941));
#6049=CARTESIAN_POINT('',(9.,8.38883057415937E-17,5.365));
#6050=CARTESIAN_POINT('Origin',(9.,1.04094977927525E-16,5.2));
#6051=CARTESIAN_POINT('',(10.,1.24301650113456E-16,5.365));
#6052=CARTESIAN_POINT('',(8.4,8.38883057415937E-17,5.365));
#6053=CARTESIAN_POINT('Origin',(10.,1.04094977927525E-16,5.2));
#6054=CARTESIAN_POINT('Origin',(9.,1.04094977927525E-16,5.2));
#6055=CARTESIAN_POINT('Origin',(8.4,1.11022302462516E-16,5.2));
#6056=CARTESIAN_POINT('',(8.4,-1.95943487863577E-16,5.1));
#6057=CARTESIAN_POINT('Origin',(8.4,0.,3.5));
#6058=CARTESIAN_POINT('Origin',(8.4,0.,3.5));
#6059=CARTESIAN_POINT('Origin',(8.4,-1.47224318643355,2.65));
#6060=CARTESIAN_POINT('',(8.4,-1.44486550797481,2.81271282285736));
#6061=CARTESIAN_POINT('',(9.,-1.44486550797481,2.81271282285736));
#6062=CARTESIAN_POINT('',(8.4,-1.44486550797481,2.81271282285736));
#6063=CARTESIAN_POINT('',(8.4,-1.31764090908823,2.59235335361323));
#6064=CARTESIAN_POINT('Origin',(8.4,-1.47224318643355,2.65));
#6065=CARTESIAN_POINT('',(9.,-1.31764090908823,2.59235335361323));
#6066=CARTESIAN_POINT('',(8.4,-1.31764090908823,2.59235335361323));
#6067=CARTESIAN_POINT('',(9.,-1.47224318643355,2.815));
#6068=CARTESIAN_POINT('Origin',(9.,-1.47224318643355,2.65));
#6069=CARTESIAN_POINT('',(10.,-1.47224318643355,2.815));
#6070=CARTESIAN_POINT('',(8.4,-1.47224318643355,2.815));
#6071=CARTESIAN_POINT('Origin',(10.,-1.47224318643355,2.65));
#6072=CARTESIAN_POINT('Origin',(9.,-1.47224318643355,2.65));
#6073=CARTESIAN_POINT('Origin',(8.4,-1.47224318643355,2.65));
#6074=CARTESIAN_POINT('Origin',(8.4,0.,3.5));
#6075=CARTESIAN_POINT('Origin',(8.4,1.47224318643355,2.65));
#6076=CARTESIAN_POINT('',(8.4,1.31764090908823,2.59235335361323));
#6077=CARTESIAN_POINT('',(9.,1.31764090908823,2.59235335361323));
#6078=CARTESIAN_POINT('',(8.4,1.31764090908823,2.59235335361323));
#6079=CARTESIAN_POINT('',(8.4,1.44486550797481,2.81271282285736));
#6080=CARTESIAN_POINT('Origin',(8.4,1.47224318643355,2.65));
#6081=CARTESIAN_POINT('',(9.,1.44486550797481,2.81271282285736));
#6082=CARTESIAN_POINT('',(8.4,1.44486550797481,2.81271282285736));
#6083=CARTESIAN_POINT('',(9.,1.47224318643355,2.815));
#6084=CARTESIAN_POINT('Origin',(9.,1.47224318643355,2.65));
#6085=CARTESIAN_POINT('',(10.,1.47224318643355,2.815));
#6086=CARTESIAN_POINT('',(8.4,1.47224318643355,2.815));
#6087=CARTESIAN_POINT('Origin',(10.,1.47224318643355,2.65));
#6088=CARTESIAN_POINT('Origin',(9.,1.47224318643355,2.65));
#6089=CARTESIAN_POINT('Origin',(8.4,1.47224318643355,2.65));
#6090=CARTESIAN_POINT('Origin',(8.4,0.,3.5));
#6091=CARTESIAN_POINT('Origin',(9.,0.,3.5));
#6092=CARTESIAN_POINT('',(9.,-2.44929359829471E-16,5.5));
#6093=CARTESIAN_POINT('Origin',(9.,0.,3.5));
#6094=CARTESIAN_POINT('Origin',(9.,0.,3.5));
#6095=CARTESIAN_POINT('Origin',(9.,0.,3.5));
#6096=CARTESIAN_POINT('Origin',(9.,0.,3.5));
#6097=CARTESIAN_POINT('Origin',(1.6,1.11022302462516E-16,5.2));
#6098=CARTESIAN_POINT('',(1.6,0.12722459888658,5.09493382352941));
#6099=CARTESIAN_POINT('',(1.6,-1.95943487863577E-16,5.1));
#6100=CARTESIAN_POINT('Origin',(1.6,0.,3.5));
#6101=CARTESIAN_POINT('',(1.6,-0.12722459888658,5.09493382352941));
#6102=CARTESIAN_POINT('Origin',(1.6,1.04094977927525E-16,5.2));
#6103=CARTESIAN_POINT('Origin',(1.6,0.,3.5));
#6104=CARTESIAN_POINT('Origin',(-0.1,1.04094977927525E-16,5.2));
#6105=CARTESIAN_POINT('',(0.,8.38883057415937E-17,5.365));
#6106=CARTESIAN_POINT('Origin',(0.,1.04094977927525E-16,5.2));
#6107=CARTESIAN_POINT('',(1.,8.38883057415937E-17,5.365));
#6108=CARTESIAN_POINT('',(-0.1,8.38883057415937E-17,5.365));
#6109=CARTESIAN_POINT('',(1.,-0.127224598886581,5.09493382352941));
#6110=CARTESIAN_POINT('Origin',(1.,1.04094977927525E-16,5.2));
#6111=CARTESIAN_POINT('',(-0.1,-0.12722459888658,5.09493382352941));
#6112=CARTESIAN_POINT('',(1.,0.127224598886581,5.09493382352941));
#6113=CARTESIAN_POINT('',(-0.1,0.12722459888658,5.09493382352941));
#6114=CARTESIAN_POINT('Origin',(1.,1.04094977927525E-16,5.2));
#6115=CARTESIAN_POINT('Origin',(1.6,-1.47224318643355,2.65));
#6116=CARTESIAN_POINT('',(1.6,-1.44486550797481,2.81271282285736));
#6117=CARTESIAN_POINT('',(1.6,-1.31764090908823,2.59235335361323));
#6118=CARTESIAN_POINT('Origin',(1.6,0.,3.5));
#6119=CARTESIAN_POINT('Origin',(1.6,-1.47224318643355,2.65));
#6120=CARTESIAN_POINT('Origin',(-0.1,-1.47224318643355,2.65));
#6121=CARTESIAN_POINT('',(0.,-1.47224318643355,2.815));
#6122=CARTESIAN_POINT('Origin',(0.,-1.47224318643355,2.65));
#6123=CARTESIAN_POINT('',(1.,-1.47224318643355,2.815));
#6124=CARTESIAN_POINT('',(-0.1,-1.47224318643355,2.815));
#6125=CARTESIAN_POINT('',(1.,-1.31764090908823,2.59235335361323));
#6126=CARTESIAN_POINT('Origin',(1.,-1.47224318643355,2.65));
#6127=CARTESIAN_POINT('',(-0.1,-1.31764090908823,2.59235335361323));
#6128=CARTESIAN_POINT('',(1.,-1.44486550797481,2.81271282285736));
#6129=CARTESIAN_POINT('',(-0.1,-1.44486550797481,2.81271282285736));
#6130=CARTESIAN_POINT('Origin',(1.,-1.47224318643355,2.65));
#6131=CARTESIAN_POINT('Origin',(1.6,1.47224318643355,2.65));
#6132=CARTESIAN_POINT('',(1.6,1.31764090908823,2.59235335361323));
#6133=CARTESIAN_POINT('',(1.6,1.44486550797481,2.81271282285736));
#6134=CARTESIAN_POINT('Origin',(1.6,0.,3.5));
#6135=CARTESIAN_POINT('Origin',(1.6,1.47224318643355,2.65));
#6136=CARTESIAN_POINT('Origin',(-0.1,1.47224318643355,2.65));
#6137=CARTESIAN_POINT('',(0.,1.47224318643355,2.815));
#6138=CARTESIAN_POINT('Origin',(0.,1.47224318643355,2.65));
#6139=CARTESIAN_POINT('',(1.,1.47224318643355,2.815));
#6140=CARTESIAN_POINT('',(-0.1,1.47224318643355,2.815));
#6141=CARTESIAN_POINT('',(1.,1.44486550797481,2.81271282285736));
#6142=CARTESIAN_POINT('Origin',(1.,1.47224318643355,2.65));
#6143=CARTESIAN_POINT('',(-0.1,1.44486550797481,2.81271282285736));
#6144=CARTESIAN_POINT('',(1.,1.31764090908823,2.59235335361323));
#6145=CARTESIAN_POINT('',(-0.1,1.31764090908823,2.59235335361323));
#6146=CARTESIAN_POINT('Origin',(1.,1.47224318643355,2.65));
#6147=CARTESIAN_POINT('Origin',(0.,0.,3.5));
#6148=CARTESIAN_POINT('',(0.,-1.95943487863577E-16,5.1));
#6149=CARTESIAN_POINT('Origin',(1.,0.,3.5));
#6150=CARTESIAN_POINT('Origin',(1.,0.,3.5));
#6151=CARTESIAN_POINT('Origin',(1.,0.,3.5));
#6152=CARTESIAN_POINT('Origin',(9.,0.,3.5));
#6153=CARTESIAN_POINT('',(10.,-2.44929359829471E-16,5.5));
#6154=CARTESIAN_POINT('Origin',(10.,0.,3.5));
#6155=CARTESIAN_POINT('',(9.,-2.44929359829471E-16,5.5));
#6156=CARTESIAN_POINT('Origin',(1.,0.,3.5));
#6157=CARTESIAN_POINT('',(1.,-2.44929359829471E-16,5.5));
#6158=CARTESIAN_POINT('Origin',(1.,0.,3.5));
#6159=CARTESIAN_POINT('Origin',(0.,0.,3.5));
#6160=CARTESIAN_POINT('',(0.,-2.44929359829471E-16,5.5));
#6161=CARTESIAN_POINT('',(0.,-2.44929359829471E-16,5.5));
#6162=CARTESIAN_POINT('Origin',(0.,0.,3.5));
#6163=CARTESIAN_POINT('Origin',(0.,0.,3.5));
#6164=CARTESIAN_POINT('',(10.,-1.28587913910472E-16,4.55));
#6165=CARTESIAN_POINT('Origin',(10.,0.,3.5));
#6166=CARTESIAN_POINT('',(0.,-1.28587913910472E-16,4.55));
#6167=CARTESIAN_POINT('',(0.,-1.28587913910472E-16,4.55));
#6168=CARTESIAN_POINT('Origin',(0.,0.,3.5));
#6169=CARTESIAN_POINT('Origin',(10.,0.,3.5));
#6170=CARTESIAN_POINT('Origin',(0.,0.,3.5));
#6171=CARTESIAN_POINT('',(0.,0.,0.));
#6172=CARTESIAN_POINT('Origin',(2.2,-2.1,2.5));
#6173=CARTESIAN_POINT('',(1.99,-2.1,2.5));
#6174=CARTESIAN_POINT('Origin',(2.2,-2.1,2.5));
#6175=CARTESIAN_POINT('',(1.99,-2.1,3.5));
#6176=CARTESIAN_POINT('',(1.99,-2.1,2.5));
#6177=CARTESIAN_POINT('Origin',(2.2,-2.1,3.5));
#6178=CARTESIAN_POINT('Origin',(2.2,-2.1,2.5));
#6179=CARTESIAN_POINT('Origin',(2.2,2.1,2.5));
#6180=CARTESIAN_POINT('',(1.99,2.1,2.5));
#6181=CARTESIAN_POINT('Origin',(2.2,2.1,2.5));
#6182=CARTESIAN_POINT('',(1.99,2.1,3.5));
#6183=CARTESIAN_POINT('',(1.99,2.1,2.5));
#6184=CARTESIAN_POINT('Origin',(2.2,2.1,3.5));
#6185=CARTESIAN_POINT('Origin',(2.2,2.1,2.5));
#6186=CARTESIAN_POINT('Origin',(2.2,-2.1,0.9));
#6187=CARTESIAN_POINT('',(1.99,-2.1,1.));
#6188=CARTESIAN_POINT('Origin',(2.2,-2.1,1.));
#6189=CARTESIAN_POINT('',(1.99,-2.1,2.3));
#6190=CARTESIAN_POINT('',(1.99,-2.1,0.9));
#6191=CARTESIAN_POINT('Origin',(2.2,-2.1,2.3));
#6192=CARTESIAN_POINT('Origin',(2.2,-2.1,2.3));
#6193=CARTESIAN_POINT('Origin',(2.2,2.1,0.9));
#6194=CARTESIAN_POINT('',(1.99,2.1,1.));
#6195=CARTESIAN_POINT('Origin',(2.2,2.1,1.));
#6196=CARTESIAN_POINT('',(1.99,2.1,2.3));
#6197=CARTESIAN_POINT('',(1.99,2.1,0.9));
#6198=CARTESIAN_POINT('Origin',(2.2,2.1,2.3));
#6199=CARTESIAN_POINT('Origin',(2.2,2.1,2.3));
#6200=CARTESIAN_POINT('Origin',(1.4,0.,3.5));
#6201=CARTESIAN_POINT('',(1.5,-1.6,3.5));
#6202=CARTESIAN_POINT('',(1.5,1.6,3.5));
#6203=CARTESIAN_POINT('Origin',(1.5,0.,3.5));
#6204=CARTESIAN_POINT('',(2.9,-1.6,3.5));
#6205=CARTESIAN_POINT('',(1.4,-1.6,3.5));
#6206=CARTESIAN_POINT('',(2.9,1.6,3.5));
#6207=CARTESIAN_POINT('Origin',(2.9,0.,3.5));
#6208=CARTESIAN_POINT('',(1.4,1.6,3.5));
#6209=CARTESIAN_POINT('Origin',(2.9,-2.5,1.));
#6210=CARTESIAN_POINT('',(2.9,-2.5,3.5));
#6211=CARTESIAN_POINT('',(2.9,-2.5,3.5));
#6212=CARTESIAN_POINT('',(2.9,-2.5,1.));
#6213=CARTESIAN_POINT('',(2.9,-2.5,1.));
#6214=CARTESIAN_POINT('',(2.9,2.5,1.));
#6215=CARTESIAN_POINT('',(2.9,-2.5,1.));
#6216=CARTESIAN_POINT('',(2.9,2.5,3.5));
#6217=CARTESIAN_POINT('',(2.9,2.5,1.));
#6218=CARTESIAN_POINT('',(2.9,-2.5,3.5));
#6219=CARTESIAN_POINT('Origin',(2.2,0.,3.5));
#6220=CARTESIAN_POINT('',(1.5,-2.5,3.5));
#6221=CARTESIAN_POINT('',(1.5,2.5,3.5));
#6222=CARTESIAN_POINT('',(1.5,-2.5,3.5));
#6223=CARTESIAN_POINT('Origin',(2.9,2.5,1.));
#6224=CARTESIAN_POINT('',(1.5,2.5,1.));
#6225=CARTESIAN_POINT('',(2.9,2.5,1.));
#6226=CARTESIAN_POINT('',(1.5,2.5,3.5));
#6227=CARTESIAN_POINT('',(1.5,2.5,1.));
#6228=CARTESIAN_POINT('',(2.9,2.5,3.5));
#6229=CARTESIAN_POINT('Origin',(1.5,-2.5,1.));
#6230=CARTESIAN_POINT('',(1.5,-2.5,1.));
#6231=CARTESIAN_POINT('',(1.5,-2.5,1.));
#6232=CARTESIAN_POINT('',(1.5,-2.5,1.));
#6233=CARTESIAN_POINT('Origin',(1.5,2.5,1.));
#6234=CARTESIAN_POINT('',(1.5,2.5,3.5));
#6235=CARTESIAN_POINT('',(1.5,2.5,1.));
#6236=CARTESIAN_POINT('Origin',(2.2,0.,3.5));
#6237=CARTESIAN_POINT('Origin',(2.2,0.,1.));
#6238=CARTESIAN_POINT('',(0.,0.,0.));
#6239=CARTESIAN_POINT('Origin',(2.2,-2.1,4.8));
#6240=CARTESIAN_POINT('',(2.45617376914899,-2.5,4.8));
#6241=CARTESIAN_POINT('',(1.94382623085101,-2.5,4.8));
#6242=CARTESIAN_POINT('',(1.85,-2.5,4.8));
#6243=CARTESIAN_POINT('Origin',(2.2,-2.1,4.8));
#6244=CARTESIAN_POINT('',(1.925,-2.1,4.8));
#6245=CARTESIAN_POINT('Origin',(2.2,-2.1,4.8));
#6246=CARTESIAN_POINT('Origin',(2.2,-2.1,4.8));
#6247=CARTESIAN_POINT('',(2.45617376914899,-2.5,5.5));
#6248=CARTESIAN_POINT('',(2.45617376914899,-2.5,4.8));
#6249=CARTESIAN_POINT('',(1.94382623085101,-2.5,5.5));
#6250=CARTESIAN_POINT('Origin',(2.2,-2.1,5.5));
#6251=CARTESIAN_POINT('',(1.94382623085101,-2.5,4.8));
#6252=CARTESIAN_POINT('Origin',(2.2,2.1,4.8));
#6253=CARTESIAN_POINT('',(1.94382623085101,2.5,4.8));
#6254=CARTESIAN_POINT('',(2.45617376914899,2.5,4.8));
#6255=CARTESIAN_POINT('',(2.55,2.5,4.8));
#6256=CARTESIAN_POINT('Origin',(2.2,2.1,4.8));
#6257=CARTESIAN_POINT('',(1.925,2.1,4.8));
#6258=CARTESIAN_POINT('Origin',(2.2,2.1,4.8));
#6259=CARTESIAN_POINT('Origin',(2.2,2.1,4.8));
#6260=CARTESIAN_POINT('',(1.94382623085101,2.5,5.5));
#6261=CARTESIAN_POINT('',(1.94382623085101,2.5,4.8));
#6262=CARTESIAN_POINT('',(2.45617376914899,2.5,5.5));
#6263=CARTESIAN_POINT('Origin',(2.2,2.1,5.5));
#6264=CARTESIAN_POINT('',(2.45617376914899,2.5,4.8));
#6265=CARTESIAN_POINT('Origin',(1.5,-2.5,3.5));
#6266=CARTESIAN_POINT('',(1.5,-2.5,5.5));
#6267=CARTESIAN_POINT('',(1.5,-2.5,5.5));
#6268=CARTESIAN_POINT('',(1.5,-2.5,3.5));
#6269=CARTESIAN_POINT('',(1.5,-2.5,3.5));
#6270=CARTESIAN_POINT('',(2.9,-2.5,3.5));
#6271=CARTESIAN_POINT('',(1.5,-2.5,3.5));
#6272=CARTESIAN_POINT('',(2.9,-2.5,5.5));
#6273=CARTESIAN_POINT('',(2.9,-2.5,3.5));
#6274=CARTESIAN_POINT('',(1.5,-2.5,5.5));
#6275=CARTESIAN_POINT('Origin',(2.9,2.5,3.5));
#6276=CARTESIAN_POINT('',(2.9,2.5,5.5));
#6277=CARTESIAN_POINT('',(2.9,2.5,5.5));
#6278=CARTESIAN_POINT('',(2.9,2.5,3.5));
#6279=CARTESIAN_POINT('',(2.9,2.5,3.5));
#6280=CARTESIAN_POINT('',(1.5,2.5,3.5));
#6281=CARTESIAN_POINT('',(2.9,2.5,3.5));
#6282=CARTESIAN_POINT('',(1.5,2.5,5.5));
#6283=CARTESIAN_POINT('',(1.5,2.5,3.5));
#6284=CARTESIAN_POINT('',(2.9,2.5,5.5));
#6285=CARTESIAN_POINT('Origin',(2.2,-2.1,3.4));
#6286=CARTESIAN_POINT('',(1.925,-2.1,3.5));
#6287=CARTESIAN_POINT('Origin',(2.2,-2.1,3.5));
#6288=CARTESIAN_POINT('',(1.925,-2.1,3.4));
#6289=CARTESIAN_POINT('Origin',(2.2,2.1,3.4));
#6290=CARTESIAN_POINT('',(1.925,2.1,3.5));
#6291=CARTESIAN_POINT('Origin',(2.2,2.1,3.5));
#6292=CARTESIAN_POINT('',(1.925,2.1,3.4));
#6293=CARTESIAN_POINT('Origin',(1.4,0.,3.5));
#6294=CARTESIAN_POINT('',(1.5,1.6,3.5));
#6295=CARTESIAN_POINT('',(1.5,-1.6,3.5));
#6296=CARTESIAN_POINT('Origin',(1.5,0.,3.5));
#6297=CARTESIAN_POINT('',(2.9,1.6,3.5));
#6298=CARTESIAN_POINT('',(1.4,1.6,3.5));
#6299=CARTESIAN_POINT('',(2.9,-1.6,3.5));
#6300=CARTESIAN_POINT('Origin',(2.9,0.,3.5));
#6301=CARTESIAN_POINT('',(1.4,-1.6,3.5));
#6302=CARTESIAN_POINT('Origin',(2.9,-2.5,3.5));
#6303=CARTESIAN_POINT('',(2.9,-2.5,3.5));
#6304=CARTESIAN_POINT('',(2.9,-2.5,5.5));
#6305=CARTESIAN_POINT('',(2.9,-2.5,3.5));
#6306=CARTESIAN_POINT('Origin',(2.2,0.,3.5));
#6307=CARTESIAN_POINT('',(1.5,2.5,3.5));
#6308=CARTESIAN_POINT('Origin',(1.5,2.5,3.5));
#6309=CARTESIAN_POINT('',(1.5,2.5,3.5));
#6310=CARTESIAN_POINT('',(1.5,2.5,5.5));
#6311=CARTESIAN_POINT('Origin',(2.2,0.,5.5));
#6312=CARTESIAN_POINT('Origin',(2.2,0.,3.5));
#6313=CARTESIAN_POINT('',(0.,0.,0.));
#6314=CARTESIAN_POINT('Origin',(7.8,-2.1,2.5));
#6315=CARTESIAN_POINT('',(7.59,-2.1,2.5));
#6316=CARTESIAN_POINT('Origin',(7.8,-2.1,2.5));
#6317=CARTESIAN_POINT('',(7.59,-2.1,3.5));
#6318=CARTESIAN_POINT('',(7.59,-2.1,2.5));
#6319=CARTESIAN_POINT('Origin',(7.8,-2.1,3.5));
#6320=CARTESIAN_POINT('Origin',(7.8,-2.1,2.5));
#6321=CARTESIAN_POINT('Origin',(7.8,2.1,2.5));
#6322=CARTESIAN_POINT('',(7.59,2.1,2.5));
#6323=CARTESIAN_POINT('Origin',(7.8,2.1,2.5));
#6324=CARTESIAN_POINT('',(7.59,2.1,3.5));
#6325=CARTESIAN_POINT('',(7.59,2.1,2.5));
#6326=CARTESIAN_POINT('Origin',(7.8,2.1,3.5));
#6327=CARTESIAN_POINT('Origin',(7.8,2.1,2.5));
#6328=CARTESIAN_POINT('Origin',(7.8,-2.1,0.9));
#6329=CARTESIAN_POINT('',(7.59,-2.1,1.));
#6330=CARTESIAN_POINT('Origin',(7.8,-2.1,1.));
#6331=CARTESIAN_POINT('',(7.59,-2.1,2.3));
#6332=CARTESIAN_POINT('',(7.59,-2.1,0.9));
#6333=CARTESIAN_POINT('Origin',(7.8,-2.1,2.3));
#6334=CARTESIAN_POINT('Origin',(7.8,-2.1,2.3));
#6335=CARTESIAN_POINT('Origin',(7.8,2.1,0.9));
#6336=CARTESIAN_POINT('',(7.59,2.1,1.));
#6337=CARTESIAN_POINT('Origin',(7.8,2.1,1.));
#6338=CARTESIAN_POINT('',(7.59,2.1,2.3));
#6339=CARTESIAN_POINT('',(7.59,2.1,0.9));
#6340=CARTESIAN_POINT('Origin',(7.8,2.1,2.3));
#6341=CARTESIAN_POINT('Origin',(7.8,2.1,2.3));
#6342=CARTESIAN_POINT('Origin',(7.,0.,3.5));
#6343=CARTESIAN_POINT('',(7.1,-1.6,3.5));
#6344=CARTESIAN_POINT('',(7.1,1.6,3.5));
#6345=CARTESIAN_POINT('Origin',(7.1,0.,3.5));
#6346=CARTESIAN_POINT('',(8.5,-1.6,3.5));
#6347=CARTESIAN_POINT('',(7.,-1.6,3.5));
#6348=CARTESIAN_POINT('',(8.5,1.6,3.5));
#6349=CARTESIAN_POINT('Origin',(8.5,0.,3.5));
#6350=CARTESIAN_POINT('',(7.,1.6,3.5));
#6351=CARTESIAN_POINT('Origin',(8.5,-2.5,1.));
#6352=CARTESIAN_POINT('',(8.5,-2.5,3.5));
#6353=CARTESIAN_POINT('',(8.5,-2.5,3.5));
#6354=CARTESIAN_POINT('',(8.5,-2.5,1.));
#6355=CARTESIAN_POINT('',(8.5,-2.5,1.));
#6356=CARTESIAN_POINT('',(8.5,2.5,1.));
#6357=CARTESIAN_POINT('',(8.5,-2.5,1.));
#6358=CARTESIAN_POINT('',(8.5,2.5,3.5));
#6359=CARTESIAN_POINT('',(8.5,2.5,1.));
#6360=CARTESIAN_POINT('',(8.5,-2.5,3.5));
#6361=CARTESIAN_POINT('Origin',(7.8,0.,3.5));
#6362=CARTESIAN_POINT('',(7.1,-2.5,3.5));
#6363=CARTESIAN_POINT('',(7.1,2.5,3.5));
#6364=CARTESIAN_POINT('',(7.1,-2.5,3.5));
#6365=CARTESIAN_POINT('Origin',(8.5,2.5,1.));
#6366=CARTESIAN_POINT('',(7.1,2.5,1.));
#6367=CARTESIAN_POINT('',(8.5,2.5,1.));
#6368=CARTESIAN_POINT('',(7.1,2.5,3.5));
#6369=CARTESIAN_POINT('',(7.1,2.5,1.));
#6370=CARTESIAN_POINT('',(8.5,2.5,3.5));
#6371=CARTESIAN_POINT('Origin',(7.1,-2.5,1.));
#6372=CARTESIAN_POINT('',(7.1,-2.5,1.));
#6373=CARTESIAN_POINT('',(7.1,-2.5,1.));
#6374=CARTESIAN_POINT('',(7.1,-2.5,1.));
#6375=CARTESIAN_POINT('Origin',(7.1,2.5,1.));
#6376=CARTESIAN_POINT('',(7.1,2.5,3.5));
#6377=CARTESIAN_POINT('',(7.1,2.5,1.));
#6378=CARTESIAN_POINT('Origin',(7.8,0.,3.5));
#6379=CARTESIAN_POINT('Origin',(7.8,0.,1.));
#6380=CARTESIAN_POINT('',(0.,0.,0.));
#6381=CARTESIAN_POINT('Origin',(7.8,-2.1,4.8));
#6382=CARTESIAN_POINT('',(8.05617376914899,-2.5,4.8));
#6383=CARTESIAN_POINT('',(7.54382623085101,-2.5,4.8));
#6384=CARTESIAN_POINT('',(7.45,-2.5,4.8));
#6385=CARTESIAN_POINT('Origin',(7.8,-2.1,4.8));
#6386=CARTESIAN_POINT('',(7.525,-2.1,4.8));
#6387=CARTESIAN_POINT('Origin',(7.8,-2.1,4.8));
#6388=CARTESIAN_POINT('Origin',(7.8,-2.1,4.8));
#6389=CARTESIAN_POINT('',(8.05617376914899,-2.5,5.5));
#6390=CARTESIAN_POINT('',(8.05617376914899,-2.5,4.8));
#6391=CARTESIAN_POINT('',(7.54382623085101,-2.5,5.5));
#6392=CARTESIAN_POINT('Origin',(7.8,-2.1,5.5));
#6393=CARTESIAN_POINT('',(7.54382623085101,-2.5,4.8));
#6394=CARTESIAN_POINT('Origin',(7.8,2.1,4.8));
#6395=CARTESIAN_POINT('',(7.54382623085101,2.5,4.8));
#6396=CARTESIAN_POINT('',(8.05617376914899,2.5,4.8));
#6397=CARTESIAN_POINT('',(8.15,2.5,4.8));
#6398=CARTESIAN_POINT('Origin',(7.8,2.1,4.8));
#6399=CARTESIAN_POINT('',(7.525,2.1,4.8));
#6400=CARTESIAN_POINT('Origin',(7.8,2.1,4.8));
#6401=CARTESIAN_POINT('Origin',(7.8,2.1,4.8));
#6402=CARTESIAN_POINT('',(7.54382623085101,2.5,5.5));
#6403=CARTESIAN_POINT('',(7.54382623085101,2.5,4.8));
#6404=CARTESIAN_POINT('',(8.05617376914899,2.5,5.5));
#6405=CARTESIAN_POINT('Origin',(7.8,2.1,5.5));
#6406=CARTESIAN_POINT('',(8.05617376914899,2.5,4.8));
#6407=CARTESIAN_POINT('Origin',(7.1,-2.5,3.5));
#6408=CARTESIAN_POINT('',(7.1,-2.5,5.5));
#6409=CARTESIAN_POINT('',(7.1,-2.5,5.5));
#6410=CARTESIAN_POINT('',(7.1,-2.5,3.5));
#6411=CARTESIAN_POINT('',(7.1,-2.5,3.5));
#6412=CARTESIAN_POINT('',(8.5,-2.5,3.5));
#6413=CARTESIAN_POINT('',(7.1,-2.5,3.5));
#6414=CARTESIAN_POINT('',(8.5,-2.5,5.5));
#6415=CARTESIAN_POINT('',(8.5,-2.5,3.5));
#6416=CARTESIAN_POINT('',(7.1,-2.5,5.5));
#6417=CARTESIAN_POINT('Origin',(8.5,2.5,3.5));
#6418=CARTESIAN_POINT('',(8.5,2.5,5.5));
#6419=CARTESIAN_POINT('',(8.5,2.5,5.5));
#6420=CARTESIAN_POINT('',(8.5,2.5,3.5));
#6421=CARTESIAN_POINT('',(8.5,2.5,3.5));
#6422=CARTESIAN_POINT('',(7.1,2.5,3.5));
#6423=CARTESIAN_POINT('',(8.5,2.5,3.5));
#6424=CARTESIAN_POINT('',(7.1,2.5,5.5));
#6425=CARTESIAN_POINT('',(7.1,2.5,3.5));
#6426=CARTESIAN_POINT('',(8.5,2.5,5.5));
#6427=CARTESIAN_POINT('Origin',(7.8,-2.1,3.4));
#6428=CARTESIAN_POINT('',(7.525,-2.1,3.5));
#6429=CARTESIAN_POINT('Origin',(7.8,-2.1,3.5));
#6430=CARTESIAN_POINT('',(7.525,-2.1,3.4));
#6431=CARTESIAN_POINT('Origin',(7.8,2.1,3.4));
#6432=CARTESIAN_POINT('',(7.525,2.1,3.5));
#6433=CARTESIAN_POINT('Origin',(7.8,2.1,3.5));
#6434=CARTESIAN_POINT('',(7.525,2.1,3.4));
#6435=CARTESIAN_POINT('Origin',(7.,0.,3.5));
#6436=CARTESIAN_POINT('',(7.1,1.6,3.5));
#6437=CARTESIAN_POINT('',(7.1,-1.6,3.5));
#6438=CARTESIAN_POINT('Origin',(7.1,0.,3.5));
#6439=CARTESIAN_POINT('',(8.5,1.6,3.5));
#6440=CARTESIAN_POINT('',(7.,1.6,3.5));
#6441=CARTESIAN_POINT('',(8.5,-1.6,3.5));
#6442=CARTESIAN_POINT('Origin',(8.5,0.,3.5));
#6443=CARTESIAN_POINT('',(7.,-1.6,3.5));
#6444=CARTESIAN_POINT('Origin',(8.5,-2.5,3.5));
#6445=CARTESIAN_POINT('',(8.5,-2.5,3.5));
#6446=CARTESIAN_POINT('',(8.5,-2.5,5.5));
#6447=CARTESIAN_POINT('',(8.5,-2.5,3.5));
#6448=CARTESIAN_POINT('Origin',(7.8,0.,3.5));
#6449=CARTESIAN_POINT('',(7.1,2.5,3.5));
#6450=CARTESIAN_POINT('Origin',(7.1,2.5,3.5));
#6451=CARTESIAN_POINT('',(7.1,2.5,3.5));
#6452=CARTESIAN_POINT('',(7.1,2.5,5.5));
#6453=CARTESIAN_POINT('Origin',(7.8,0.,5.5));
#6454=CARTESIAN_POINT('Origin',(7.8,0.,3.5));
#6455=CARTESIAN_POINT('',(0.,0.,0.));
#6456=CARTESIAN_POINT('Origin',(4.,0.,3.5));
#6457=CARTESIAN_POINT('',(6.,-8.57252759403147E-17,4.2));
#6458=CARTESIAN_POINT('Origin',(6.,0.,3.5));
#6459=CARTESIAN_POINT('',(4.,-8.57252759403147E-17,4.2));
#6460=CARTESIAN_POINT('',(4.,-8.57252759403147E-17,4.2));
#6461=CARTESIAN_POINT('Origin',(4.,0.,3.5));
#6462=CARTESIAN_POINT('Origin',(4.,0.,3.5));
#6463=CARTESIAN_POINT('',(6.,-1.27363267111325E-16,4.54));
#6464=CARTESIAN_POINT('Origin',(6.,0.,3.5));
#6465=CARTESIAN_POINT('',(4.,-1.27363267111325E-16,4.54));
#6466=CARTESIAN_POINT('',(4.,-1.27363267111325E-16,4.54));
#6467=CARTESIAN_POINT('Origin',(4.,0.,3.5));
#6468=CARTESIAN_POINT('Origin',(6.,0.,3.5));
#6469=CARTESIAN_POINT('Origin',(4.,0.,3.5));
#6470=CARTESIAN_POINT('',(0.,0.,0.));
#6471=CARTESIAN_POINT('Origin',(0.,0.,3.5));
#6472=CARTESIAN_POINT('',(1.,-8.57252759403147E-17,4.2));
#6473=CARTESIAN_POINT('Origin',(1.,0.,3.5));
#6474=CARTESIAN_POINT('',(0.,-8.57252759403147E-17,4.2));
#6475=CARTESIAN_POINT('',(0.,-8.57252759403147E-17,4.2));
#6476=CARTESIAN_POINT('Origin',(0.,0.,3.5));
#6477=CARTESIAN_POINT('Origin',(0.,0.,3.5));
#6478=CARTESIAN_POINT('',(1.,-1.27363267111325E-16,4.54));
#6479=CARTESIAN_POINT('Origin',(1.,0.,3.5));
#6480=CARTESIAN_POINT('',(0.,-1.27363267111325E-16,4.54));
#6481=CARTESIAN_POINT('',(0.,-1.27363267111325E-16,4.54));
#6482=CARTESIAN_POINT('Origin',(0.,0.,3.5));
#6483=CARTESIAN_POINT('Origin',(1.,0.,3.5));
#6484=CARTESIAN_POINT('Origin',(0.,0.,3.5));
#6485=CARTESIAN_POINT('',(0.,0.,0.));
#6486=CARTESIAN_POINT('Origin',(9.,0.,3.5));
#6487=CARTESIAN_POINT('',(10.,-8.57252759403147E-17,4.2));
#6488=CARTESIAN_POINT('Origin',(10.,0.,3.5));
#6489=CARTESIAN_POINT('',(9.,-8.57252759403147E-17,4.2));
#6490=CARTESIAN_POINT('',(9.,-8.57252759403147E-17,4.2));
#6491=CARTESIAN_POINT('Origin',(9.,0.,3.5));
#6492=CARTESIAN_POINT('Origin',(9.,0.,3.5));
#6493=CARTESIAN_POINT('',(10.,-1.27363267111325E-16,4.54));
#6494=CARTESIAN_POINT('Origin',(10.,0.,3.5));
#6495=CARTESIAN_POINT('',(9.,-1.27363267111325E-16,4.54));
#6496=CARTESIAN_POINT('',(9.,-1.27363267111325E-16,4.54));
#6497=CARTESIAN_POINT('Origin',(9.,0.,3.5));
#6498=CARTESIAN_POINT('Origin',(10.,0.,3.5));
#6499=CARTESIAN_POINT('Origin',(9.,0.,3.5));
#6500=CARTESIAN_POINT('',(0.,0.,0.));
#6501=CARTESIAN_POINT('Origin',(-0.6,1.04094977927525E-16,5.2));
#6502=CARTESIAN_POINT('',(-0.5,7.65404249467096E-17,5.425));
#6503=CARTESIAN_POINT('Origin',(-0.5,1.04094977927525E-16,5.2));
#6504=CARTESIAN_POINT('',(0.,1.3164953090834E-16,5.425));
#6505=CARTESIAN_POINT('',(-0.6,7.65404249467096E-17,5.425));
#6506=CARTESIAN_POINT('Origin',(0.,1.04094977927525E-16,5.2));
#6507=CARTESIAN_POINT('Origin',(-0.6,-1.47224318643355,2.65));
#6508=CARTESIAN_POINT('',(-0.5,-1.47224318643355,2.875));
#6509=CARTESIAN_POINT('Origin',(-0.5,-1.47224318643355,2.65));
#6510=CARTESIAN_POINT('',(0.,-1.47224318643355,2.875));
#6511=CARTESIAN_POINT('',(-0.6,-1.47224318643355,2.875));
#6512=CARTESIAN_POINT('Origin',(0.,-1.47224318643355,2.65));
#6513=CARTESIAN_POINT('Origin',(-0.6,1.47224318643355,2.65));
#6514=CARTESIAN_POINT('',(-0.5,1.47224318643355,2.875));
#6515=CARTESIAN_POINT('Origin',(-0.5,1.47224318643355,2.65));
#6516=CARTESIAN_POINT('',(0.,1.47224318643355,2.875));
#6517=CARTESIAN_POINT('',(-0.6,1.47224318643355,2.875));
#6518=CARTESIAN_POINT('Origin',(0.,1.47224318643355,2.65));
#6519=CARTESIAN_POINT('Origin',(-0.9,0.,3.5));
#6520=CARTESIAN_POINT('',(-0.5,-1.34711147906209E-16,4.6));
#6521=CARTESIAN_POINT('Origin',(-0.5,0.,3.5));
#6522=CARTESIAN_POINT('',(-0.9,-1.34711147906209E-16,4.6));
#6523=CARTESIAN_POINT('',(-0.9,-1.34711147906209E-16,4.6));
#6524=CARTESIAN_POINT('Origin',(-0.9,0.,3.5));
#6525=CARTESIAN_POINT('Origin',(-0.9,0.,3.5));
#6526=CARTESIAN_POINT('',(-0.9,-8.57252759403147E-17,4.2));
#6527=CARTESIAN_POINT('Origin',(-0.9,0.,3.5));
#6528=CARTESIAN_POINT('Origin',(-0.5,0.,3.5));
#6529=CARTESIAN_POINT('',(0.,-8.57252759403147E-17,4.2));
#6530=CARTESIAN_POINT('Origin',(0.,0.,3.5));
#6531=CARTESIAN_POINT('',(-0.5,-8.57252759403147E-17,4.2));
#6532=CARTESIAN_POINT('Origin',(-0.5,0.,3.5));
#6533=CARTESIAN_POINT('',(0.,-2.44929359829471E-16,5.5));
#6534=CARTESIAN_POINT('Origin',(0.,0.,3.5));
#6535=CARTESIAN_POINT('',(-0.5,-2.44929359829471E-16,5.5));
#6536=CARTESIAN_POINT('',(-0.5,-2.44929359829471E-16,5.5));
#6537=CARTESIAN_POINT('Origin',(-0.5,0.,3.5));
#6538=CARTESIAN_POINT('Origin',(0.,0.,3.5));
#6539=CARTESIAN_POINT('Origin',(-0.5,0.,3.5));
#6540=CARTESIAN_POINT('',(0.,0.,0.));
#6541=CARTESIAN_POINT('Origin',(11.,1.1,4.65));
#6542=CARTESIAN_POINT('',(11.1785346780556,0.963068014212911,4.65));
#6543=CARTESIAN_POINT('',(10.8214653219444,0.963068014212911,4.65));
#6544=CARTESIAN_POINT('',(10.5,0.963068014212911,4.65));
#6545=CARTESIAN_POINT('Origin',(11.,1.1,4.65));
#6546=CARTESIAN_POINT('Origin',(11.,1.1,3.65));
#6547=CARTESIAN_POINT('',(10.775,1.1,3.65));
#6548=CARTESIAN_POINT('Origin',(11.,1.1,3.65));
#6549=CARTESIAN_POINT('',(10.775,1.09999999957979,4.51980390362508));
#6550=CARTESIAN_POINT('',(10.775,1.1,3.65));
#6551=CARTESIAN_POINT('Ctrl Pts',(10.8214653219444,0.963068014212911,4.65));
#6552=CARTESIAN_POINT('Ctrl Pts',(10.8162688127795,0.969843327412709,4.6443260109313));
#6553=CARTESIAN_POINT('Ctrl Pts',(10.8115201211091,0.976836537416272,4.63836687623802));
#6554=CARTESIAN_POINT('Ctrl Pts',(10.792918343781,1.0077339139021,4.61151493738561));
#6555=CARTESIAN_POINT('Ctrl Pts',(10.7840010147256,1.03286247939125,4.58821848420302));
#6556=CARTESIAN_POINT('Ctrl Pts',(10.7764275645432,1.07048803422142,4.55094929145805));
#6557=CARTESIAN_POINT('Ctrl Pts',(10.7750000000547,1.08535718524001,4.53559821000295));
#6558=CARTESIAN_POINT('Ctrl Pts',(10.775,1.09999999915957,4.51980390362508));
#6559=CARTESIAN_POINT('Ctrl Pts',(10.775,1.09999999915957,4.51980390362508));
#6560=CARTESIAN_POINT('Ctrl Pts',(10.7749999998623,1.13686223670398,4.48004286611214));
#6561=CARTESIAN_POINT('Ctrl Pts',(10.7839934300633,1.17220221216353,4.4373912158357));
#6562=CARTESIAN_POINT('Ctrl Pts',(10.8116025036461,1.22546035116394,4.36579074537975));
#6563=CARTESIAN_POINT('Ctrl Pts',(10.826392404746,1.24536021423858,4.33673835178744));
#6564=CARTESIAN_POINT('Ctrl Pts',(10.8631377994706,1.28038279168244,4.28209526166438));
#6565=CARTESIAN_POINT('Ctrl Pts',(10.8846693973938,1.29561277550653,4.25628935065431));
#6566=CARTESIAN_POINT('Ctrl Pts',(10.9246244306808,1.31237665040526,4.22647603162929));
#6567=CARTESIAN_POINT('Ctrl Pts',(10.9385046923607,1.3169746204353,4.21806846608269));
#6568=CARTESIAN_POINT('Ctrl Pts',(10.9684801775212,1.32330731829159,4.20633010315014));
#6569=CARTESIAN_POINT('Ctrl Pts',(10.9846306282398,1.325,4.20311805552126));
#6570=CARTESIAN_POINT('Ctrl Pts',(11.0153693717602,1.325,4.20311805552126));
#6571=CARTESIAN_POINT('Ctrl Pts',(11.0315198224788,1.32330731829159,4.20633010315014));
#6572=CARTESIAN_POINT('Ctrl Pts',(11.0614953076393,1.3169746204353,4.21806846608269));
#6573=CARTESIAN_POINT('Ctrl Pts',(11.0753755693192,1.31237665040526,4.22647603162929));
#6574=CARTESIAN_POINT('Ctrl Pts',(11.1153306026062,1.29561277550653,4.25628935065431));
#6575=CARTESIAN_POINT('Ctrl Pts',(11.1368622005294,1.28038279168244,4.28209526166438));
#6576=CARTESIAN_POINT('Ctrl Pts',(11.173607595254,1.24536021423858,4.33673835178744));
#6577=CARTESIAN_POINT('Ctrl Pts',(11.1883974963539,1.22546035116394,4.36579074537975));
#6578=CARTESIAN_POINT('Ctrl Pts',(11.222463106795,1.15974749736021,4.45413538782613));
#6579=CARTESIAN_POINT('Ctrl Pts',(11.2311157805594,1.10796402441359,4.51382824678284));
#6580=CARTESIAN_POINT('Ctrl Pts',(11.2159989852744,1.03286247939125,4.58821848420302));
#6581=CARTESIAN_POINT('Ctrl Pts',(11.207081656219,1.0077339139021,4.61151493738561));
#6582=CARTESIAN_POINT('Ctrl Pts',(11.1884798788909,0.976836537416272,4.63836687623803));
#6583=CARTESIAN_POINT('Ctrl Pts',(11.1837311872205,0.969843327412708,4.64432601093131));
#6584=CARTESIAN_POINT('Ctrl Pts',(11.1785346780556,0.963068014212911,4.65));
#6585=CARTESIAN_POINT('Origin',(11.,1.1,2.3));
#6586=CARTESIAN_POINT('',(11.,0.935000000000001,2.32706564548565));
#6587=CARTESIAN_POINT('',(10.835,1.1,2.48019609728144));
#6588=CARTESIAN_POINT('Ctrl Pts',(11.,0.935000000000001,2.32706564548565));
#6589=CARTESIAN_POINT('Ctrl Pts',(11.0202396786782,0.935000000000001,2.32706564548565));
#6590=CARTESIAN_POINT('Ctrl Pts',(11.0413998843664,0.938976037222427,2.33020641131557));
#6591=CARTESIAN_POINT('Ctrl Pts',(11.079434847611,0.953942593189685,2.34237891599741));
#6592=CARTESIAN_POINT('Ctrl Pts',(11.0963248656201,0.964885450235815,2.35142151909605));
#6593=CARTESIAN_POINT('Ctrl Pts',(11.1285584673749,0.993474390588197,2.3759424605798));
#6594=CARTESIAN_POINT('Ctrl Pts',(11.142996001906,1.01439122017948,2.39460099158616));
#6595=CARTESIAN_POINT('Ctrl Pts',(11.161205098565,1.0576959560997,2.43596250694638));
#6596=CARTESIAN_POINT('Ctrl Pts',(11.165,1.08005630656369,2.45868405685733));
#6597=CARTESIAN_POINT('Ctrl Pts',(11.165,1.12307636456025,2.50508715814972));
#6598=CARTESIAN_POINT('Ctrl Pts',(11.1599788863536,1.14709181073674,2.53283337360734));
#6599=CARTESIAN_POINT('Ctrl Pts',(11.1397130351965,1.19105576310235,2.58752146760594));
#6600=CARTESIAN_POINT('Ctrl Pts',(11.1246027452831,1.21104555821498,2.61447988461167));
#6601=CARTESIAN_POINT('Ctrl Pts',(11.0931318205307,1.23710826004727,2.65155012736531));
#6602=CARTESIAN_POINT('Ctrl Pts',(11.0776964270187,1.24683112690748,2.6659894549942));
#6603=CARTESIAN_POINT('Ctrl Pts',(11.0507603369974,1.25729325232077,2.68192051821757));
#6604=CARTESIAN_POINT('Ctrl Pts',(11.0411497301163,1.2601136995706,2.68628885375725));
#6605=CARTESIAN_POINT('Ctrl Pts',(11.0210767897834,1.26396632271753,2.69228583186432));
#6606=CARTESIAN_POINT('Ctrl Pts',(11.0106145359623,1.265,2.69391377632414));
#6607=CARTESIAN_POINT('Ctrl Pts',(10.9893854640377,1.265,2.69391377632414));
#6608=CARTESIAN_POINT('Ctrl Pts',(10.9789232102166,1.26396632271753,2.69228583186432));
#6609=CARTESIAN_POINT('Ctrl Pts',(10.9588502698837,1.2601136995706,2.68628885375725));
#6610=CARTESIAN_POINT('Ctrl Pts',(10.9492396630026,1.25729325232077,2.68192051821757));
#6611=CARTESIAN_POINT('Ctrl Pts',(10.9223035729813,1.24683112690748,2.6659894549942));
#6612=CARTESIAN_POINT('Ctrl Pts',(10.9068681794693,1.23710826004727,2.65155012736531));
#6613=CARTESIAN_POINT('Ctrl Pts',(10.8753972547169,1.21104555821498,2.61447988461167));
#6614=CARTESIAN_POINT('Ctrl Pts',(10.8602869648035,1.19105576310235,2.58752146760594));
#6615=CARTESIAN_POINT('Ctrl Pts',(10.8400211136464,1.14709181073674,2.53283337360734));
#6616=CARTESIAN_POINT('Ctrl Pts',(10.835,1.12307636456025,2.50508715814972));
#6617=CARTESIAN_POINT('Ctrl Pts',(10.835,1.1,2.48019609728144));
#6618=CARTESIAN_POINT('Ctrl Pts',(10.835,1.1,2.48019609728144));
#6619=CARTESIAN_POINT('Ctrl Pts',(10.835,1.08005630656369,2.45868405685733));
#6620=CARTESIAN_POINT('Ctrl Pts',(10.838794901435,1.0576959560997,2.43596250694638));
#6621=CARTESIAN_POINT('Ctrl Pts',(10.857003998094,1.01439122017948,2.39460099158616));
#6622=CARTESIAN_POINT('Ctrl Pts',(10.8714415326251,0.993474390588197,2.3759424605798));
#6623=CARTESIAN_POINT('Ctrl Pts',(10.9036751343799,0.964885450235815,2.35142151909605));
#6624=CARTESIAN_POINT('Ctrl Pts',(10.920565152389,0.953942593189685,2.34237891599741));
#6625=CARTESIAN_POINT('Ctrl Pts',(10.9586001156336,0.938976037222427,2.33020641131557));
#6626=CARTESIAN_POINT('Ctrl Pts',(10.9797603213218,0.935000000000001,2.32706564548565));
#6627=CARTESIAN_POINT('Ctrl Pts',(11.,0.935000000000001,2.32706564548565));
#6628=CARTESIAN_POINT('',(10.835,1.1,3.35));
#6629=CARTESIAN_POINT('',(10.835,1.1,2.3));
#6630=CARTESIAN_POINT('Origin',(11.,1.1,3.35));
#6631=CARTESIAN_POINT('Origin',(10.6,1.11022302462516E-16,5.2));
#6632=CARTESIAN_POINT('',(10.6,0.0967741410450116,4.996875));
#6633=CARTESIAN_POINT('',(10.6,-0.0967741410450114,4.996875));
#6634=CARTESIAN_POINT('Origin',(10.6,0.,3.5));
#6635=CARTESIAN_POINT('Origin',(10.6,1.04094977927525E-16,5.2));
#6636=CARTESIAN_POINT('Origin',(9.9,1.04094977927525E-16,5.2));
#6637=CARTESIAN_POINT('',(10.,7.65404249467096E-17,5.425));
#6638=CARTESIAN_POINT('Origin',(10.,1.04094977927525E-16,5.2));
#6639=CARTESIAN_POINT('',(10.5,7.65404249467096E-17,5.425));
#6640=CARTESIAN_POINT('',(9.9,7.65404249467096E-17,5.425));
#6641=CARTESIAN_POINT('',(10.5,-0.0967741410450087,4.996875));
#6642=CARTESIAN_POINT('Origin',(10.5,1.04094977927525E-16,5.2));
#6643=CARTESIAN_POINT('',(9.9,-0.0967741410450114,4.996875));
#6644=CARTESIAN_POINT('',(10.5,0.0967741410450089,4.996875));
#6645=CARTESIAN_POINT('',(9.9,0.0967741410450116,4.996875));
#6646=CARTESIAN_POINT('Origin',(10.5,1.04094977927525E-16,5.2));
#6647=CARTESIAN_POINT('Origin',(10.6,-1.47224318643355,2.65));
#6648=CARTESIAN_POINT('',(10.6,-1.34471884681234,2.8353713645744));
#6649=CARTESIAN_POINT('',(10.6,-1.24794470576733,2.6677536354256));
#6650=CARTESIAN_POINT('Origin',(10.6,0.,3.5));
#6651=CARTESIAN_POINT('Origin',(10.6,-1.47224318643355,2.65));
#6652=CARTESIAN_POINT('Origin',(9.9,-1.47224318643355,2.65));
#6653=CARTESIAN_POINT('',(10.,-1.47224318643355,2.875));
#6654=CARTESIAN_POINT('Origin',(10.,-1.47224318643355,2.65));
#6655=CARTESIAN_POINT('',(10.5,-1.47224318643355,2.875));
#6656=CARTESIAN_POINT('',(9.9,-1.47224318643355,2.875));
#6657=CARTESIAN_POINT('',(10.5,-1.24794470576732,2.6677536354256));
#6658=CARTESIAN_POINT('Origin',(10.5,-1.47224318643355,2.65));
#6659=CARTESIAN_POINT('',(9.9,-1.24794470576733,2.6677536354256));
#6660=CARTESIAN_POINT('',(10.5,-1.34471884681234,2.8353713645744));
#6661=CARTESIAN_POINT('',(9.9,-1.34471884681234,2.8353713645744));
#6662=CARTESIAN_POINT('Origin',(10.5,-1.47224318643355,2.65));
#6663=CARTESIAN_POINT('Origin',(10.6,1.47224318643355,2.65));
#6664=CARTESIAN_POINT('',(10.6,1.24794470576732,2.6677536354256));
#6665=CARTESIAN_POINT('',(10.6,1.34471884681234,2.8353713645744));
#6666=CARTESIAN_POINT('Origin',(10.6,0.,3.5));
#6667=CARTESIAN_POINT('Origin',(10.6,1.47224318643355,2.65));
#6668=CARTESIAN_POINT('Origin',(9.9,1.47224318643355,2.65));
#6669=CARTESIAN_POINT('',(10.,1.47224318643355,2.875));
#6670=CARTESIAN_POINT('Origin',(10.,1.47224318643355,2.65));
#6671=CARTESIAN_POINT('',(10.5,1.47224318643355,2.875));
#6672=CARTESIAN_POINT('',(9.9,1.47224318643355,2.875));
#6673=CARTESIAN_POINT('',(10.5,1.34471884681234,2.8353713645744));
#6674=CARTESIAN_POINT('Origin',(10.5,1.47224318643355,2.65));
#6675=CARTESIAN_POINT('',(9.9,1.34471884681234,2.8353713645744));
#6676=CARTESIAN_POINT('',(10.5,1.24794470576732,2.6677536354256));
#6677=CARTESIAN_POINT('',(9.9,1.24794470576732,2.6677536354256));
#6678=CARTESIAN_POINT('Origin',(10.5,1.47224318643355,2.65));
#6679=CARTESIAN_POINT('Origin',(10.5,0.,3.5));
#6680=CARTESIAN_POINT('Origin',(10.5,0.,3.5));
#6681=CARTESIAN_POINT('Origin',(10.5,0.,3.5));
#6682=CARTESIAN_POINT('',(10.5,1.49248115565993,3.35));
#6683=CARTESIAN_POINT('Origin',(10.5,0.,3.5));
#6684=CARTESIAN_POINT('',(11.5,1.49248115565993,3.35));
#6685=CARTESIAN_POINT('',(10.5,1.49248115565993,3.35));
#6686=CARTESIAN_POINT('',(11.5,1.49248115565993,3.65));
#6687=CARTESIAN_POINT('Origin',(11.5,0.,3.5));
#6688=CARTESIAN_POINT('',(10.5,1.49248115565993,3.65));
#6689=CARTESIAN_POINT('',(10.5,1.49248115565993,3.65));
#6690=CARTESIAN_POINT('Origin',(10.5,0.,3.5));
#6691=CARTESIAN_POINT('Origin',(10.5,1.6,3.65));
#6692=CARTESIAN_POINT('',(10.5,0.591269819963779,3.65));
#6693=CARTESIAN_POINT('',(11.5,0.591269819963779,3.65));
#6694=CARTESIAN_POINT('',(10.,0.591269819963779,3.65));
#6695=CARTESIAN_POINT('',(10.5,1.6,3.65));
#6696=CARTESIAN_POINT('',(11.5,0.8,3.65));
#6697=CARTESIAN_POINT('Origin',(10.5,0.,3.35));
#6698=CARTESIAN_POINT('',(11.5,0.591269819963779,3.35));
#6699=CARTESIAN_POINT('',(10.5,0.591269819963779,3.35));
#6700=CARTESIAN_POINT('',(10.,0.591269819963779,3.35));
#6701=CARTESIAN_POINT('',(11.5,0.,3.35));
#6702=CARTESIAN_POINT('',(10.5,0.,3.35));
#6703=CARTESIAN_POINT('Origin',(10.5,0.,3.5));
#6704=CARTESIAN_POINT('',(10.5,-2.44929359829471E-16,5.5));
#6705=CARTESIAN_POINT('Origin',(10.5,0.,3.5));
#6706=CARTESIAN_POINT('Origin',(10.5,0.,3.5));
#6707=CARTESIAN_POINT('Origin',(11.5,0.,3.5));
#6708=CARTESIAN_POINT('',(11.5,-7.47034547479885E-17,4.11));
#6709=CARTESIAN_POINT('Origin',(11.5,0.,3.5));
#6710=CARTESIAN_POINT('Origin',(11.5,0.,3.5));
#6711=CARTESIAN_POINT('Origin',(10.,0.,3.5));
#6712=CARTESIAN_POINT('',(10.,-7.47034547479885E-17,4.11));
#6713=CARTESIAN_POINT('',(10.,-7.47034547479885E-17,4.11));
#6714=CARTESIAN_POINT('Origin',(10.,0.,3.5));
#6715=CARTESIAN_POINT('Origin',(10.,0.,3.5));
#6716=CARTESIAN_POINT('',(10.,-2.44929359829471E-16,5.5));
#6717=CARTESIAN_POINT('',(10.,-2.44929359829471E-16,5.5));
#6718=CARTESIAN_POINT('Origin',(10.,0.,3.5));
#6719=CARTESIAN_POINT('Origin',(10.,0.,3.5));
#6720=CARTESIAN_POINT('',(0.,0.,0.));
#6721=CARTESIAN_POINT('Origin',(0.375,0.5,0.));
#6722=CARTESIAN_POINT('',(-0.375,0.5,-4.59242549680257E-17));
#6723=CARTESIAN_POINT('Origin',(0.,0.5,0.));
#6724=CARTESIAN_POINT('Origin',(0.,0.475,0.));
#6725=CARTESIAN_POINT('',(-0.425,0.45,-5.20474889637625E-17));
#6726=CARTESIAN_POINT('Origin',(0.,0.45,0.));
#6727=CARTESIAN_POINT('',(-0.4,0.475,-4.89858719658941E-17));
#6728=CARTESIAN_POINT('Origin',(0.,0.24,0.));
#6729=CARTESIAN_POINT('',(-0.425,0.0299999999999998,-5.20474889637625E-17));
#6730=CARTESIAN_POINT('Origin',(0.,0.0299999999999998,0.));
#6731=CARTESIAN_POINT('',(-0.425,0.24,-5.20474889637625E-17));
#6732=CARTESIAN_POINT('Origin',(0.,0.0150000000000001,0.));
#6733=CARTESIAN_POINT('',(-0.395,4.85722573273506E-17,-4.83735485663204E-17));
#6734=CARTESIAN_POINT('Origin',(0.,0.,0.));
#6735=CARTESIAN_POINT('',(-0.41,0.0150000000000001,-5.02105187650415E-17));
#6736=CARTESIAN_POINT('Origin',(0.27,0.,0.));
#6737=CARTESIAN_POINT('',(-0.27,0.,-3.30654635769785E-17));
#6738=CARTESIAN_POINT('Origin',(0.,0.,0.));
#6739=CARTESIAN_POINT('Origin',(0.,-0.02,0.));
#6740=CARTESIAN_POINT('',(-0.24505,-0.0498999999999999,3.00099698131059E-17));
#6741=CARTESIAN_POINT('Origin',(0.,-0.0498999999999999,0.));
#6742=CARTESIAN_POINT('',(-0.26,-0.02,-3.18408167778312E-17));
#6743=CARTESIAN_POINT('Origin',(0.,-0.995,0.));
#6744=CARTESIAN_POINT('',(-0.24505,-1.95495,3.00099698131059E-17));
#6745=CARTESIAN_POINT('Origin',(0.,-1.95495,0.));
#6746=CARTESIAN_POINT('',(-0.24505,-0.995,-3.00099698131059E-17));
#6747=CARTESIAN_POINT('Origin',(0.,-1.975,0.));
#6748=CARTESIAN_POINT('',(-0.2,-2.,-2.44929359829471E-17));
#6749=CARTESIAN_POINT('Origin',(0.,-2.,0.));
#6750=CARTESIAN_POINT('',(-0.225,-1.975,-2.75545529808154E-17));
#6751=CARTESIAN_POINT('Origin',(0.,-2.,0.));
#6752=CARTESIAN_POINT('Origin',(0.115470053837925,-0.5,-0.2));
#6753=CARTESIAN_POINT('',(0.23094010767585,-0.5,0.));
#6754=CARTESIAN_POINT('',(0.115470053837925,-0.5,-0.2));
#6755=CARTESIAN_POINT('',(0.23094010767585,-0.5,0.));
#6756=CARTESIAN_POINT('',(0.115470053837925,-0.8,-0.2));
#6757=CARTESIAN_POINT('',(0.115470053837925,-0.5,-0.2));
#6758=CARTESIAN_POINT('',(0.23094010767585,-0.8,0.));
#6759=CARTESIAN_POINT('',(0.23094010767585,-0.8,0.));
#6760=CARTESIAN_POINT('',(0.23094010767585,-0.5,0.));
#6761=CARTESIAN_POINT('Origin',(-0.115470053837925,-0.5,-0.2));
#6762=CARTESIAN_POINT('',(-0.115470053837925,-0.5,-0.2));
#6763=CARTESIAN_POINT('',(0.115470053837925,-0.5,-0.2));
#6764=CARTESIAN_POINT('',(-0.115470053837925,-0.8,-0.2));
#6765=CARTESIAN_POINT('',(-0.115470053837925,-0.5,-0.2));
#6766=CARTESIAN_POINT('',(0.115470053837925,-0.8,-0.2));
#6767=CARTESIAN_POINT('Origin',(-0.23094010767585,-0.5,-2.77555756156289E-17));
#6768=CARTESIAN_POINT('',(-0.23094010767585,-0.5,-2.82820063659975E-17));
#6769=CARTESIAN_POINT('',(-0.115470053837925,-0.5,-0.2));
#6770=CARTESIAN_POINT('',(-0.23094010767585,-0.8,-2.77555756156289E-17));
#6771=CARTESIAN_POINT('',(-0.23094010767585,-0.5,-2.82820063659975E-17));
#6772=CARTESIAN_POINT('',(-0.115470053837925,-0.8,-0.2));
#6773=CARTESIAN_POINT('Origin',(-0.115470053837925,-0.5,0.2));
#6774=CARTESIAN_POINT('',(-0.115470053837925,-0.5,0.2));
#6775=CARTESIAN_POINT('',(-0.23094010767585,-0.5,-2.82820063659975E-17));
#6776=CARTESIAN_POINT('',(-0.115470053837925,-0.8,0.2));
#6777=CARTESIAN_POINT('',(-0.115470053837925,-0.5,0.2));
#6778=CARTESIAN_POINT('',(-0.23094010767585,-0.8,-2.82820063659975E-17));
#6779=CARTESIAN_POINT('Origin',(0.115470053837925,-0.5,0.2));
#6780=CARTESIAN_POINT('',(0.115470053837925,-0.5,0.2));
#6781=CARTESIAN_POINT('',(-0.115470053837925,-0.5,0.2));
#6782=CARTESIAN_POINT('',(0.115470053837925,-0.8,0.2));
#6783=CARTESIAN_POINT('',(0.115470053837925,-0.5,0.2));
#6784=CARTESIAN_POINT('',(-0.115470053837925,-0.8,0.2));
#6785=CARTESIAN_POINT('Origin',(0.23094010767585,-0.5,0.));
#6786=CARTESIAN_POINT('',(0.115470053837925,-0.5,0.2));
#6787=CARTESIAN_POINT('',(0.115470053837925,-0.8,0.2));
#6788=CARTESIAN_POINT('Origin',(0.,-0.5,0.));
#6789=CARTESIAN_POINT('Origin',(0.,-0.8,0.));
#6790=CARTESIAN_POINT('',(0.,0.,0.));
#6791=CARTESIAN_POINT('',(0.,0.,0.));
#6792=CARTESIAN_POINT('Origin',(0.75,1.2,0.));
#6793=CARTESIAN_POINT('',(0.885663593019381,1.2,-0.16));
#6794=CARTESIAN_POINT('',(0.885663593019381,1.2,0.16));
#6795=CARTESIAN_POINT('Origin',(0.,1.2,0.));
#6796=CARTESIAN_POINT('',(0.93,1.2,-0.16));
#6797=CARTESIAN_POINT('',(0.93,1.2,-0.16));
#6798=CARTESIAN_POINT('',(0.93,1.2,0.16));
#6799=CARTESIAN_POINT('',(0.93,1.2,0.16));
#6800=CARTESIAN_POINT('',(0.57,1.2,0.16));
#6801=CARTESIAN_POINT('Origin',(0.57,0.,0.16));
#6802=CARTESIAN_POINT('',(0.885663593019381,-1.2,0.16));
#6803=CARTESIAN_POINT('',(0.885663593019381,0.,0.16));
#6804=CARTESIAN_POINT('',(0.93,-1.2,0.16));
#6805=CARTESIAN_POINT('',(0.93,0.,0.16));
#6806=CARTESIAN_POINT('',(0.57,-1.2,0.16));
#6807=CARTESIAN_POINT('Origin',(0.75,-1.2,0.));
#6808=CARTESIAN_POINT('',(0.885663593019381,-1.2,-0.16));
#6809=CARTESIAN_POINT('Origin',(0.,-1.2,0.));
#6810=CARTESIAN_POINT('',(0.93,-1.2,-0.16));
#6811=CARTESIAN_POINT('',(0.93,-1.2,0.16));
#6812=CARTESIAN_POINT('',(0.93,-1.2,-0.16));
#6813=CARTESIAN_POINT('Origin',(0.93,0.,-0.16));
#6814=CARTESIAN_POINT('',(0.885663593019381,0.,-0.16));
#6815=CARTESIAN_POINT('',(0.93,0.,-0.16));
#6816=CARTESIAN_POINT('Origin',(0.93,0.,0.16));
#6817=CARTESIAN_POINT('Origin',(1.05,1.5,0.));
#6818=CARTESIAN_POINT('',(-1.05,1.5,-1.28587913910472E-16));
#6819=CARTESIAN_POINT('Origin',(0.,1.5,0.));
#6820=CARTESIAN_POINT('',(-0.9,1.5,-1.10218211923262E-16));
#6821=CARTESIAN_POINT('Origin',(0.,1.5,0.));
#6822=CARTESIAN_POINT('Origin',(0.,1.315,0.));
#6823=CARTESIAN_POINT('',(-1.05,1.13,-1.28587913910472E-16));
#6824=CARTESIAN_POINT('Origin',(0.,1.13,0.));
#6825=CARTESIAN_POINT('',(-1.05,1.315,-1.28587913910472E-16));
#6826=CARTESIAN_POINT('Origin',(1.,1.13,0.));
#6827=CARTESIAN_POINT('',(-1.,1.13,-1.22464679914735E-16));
#6828=CARTESIAN_POINT('Origin',(0.,1.13,0.));
#6829=CARTESIAN_POINT('Origin',(0.,1.065,0.));
#6830=CARTESIAN_POINT('',(-1.,1.,-1.22464679914735E-16));
#6831=CARTESIAN_POINT('Origin',(0.,1.,0.));
#6832=CARTESIAN_POINT('',(-1.,1.065,-1.22464679914735E-16));
#6833=CARTESIAN_POINT('Origin',(1.05,1.,0.));
#6834=CARTESIAN_POINT('',(-1.05,1.,-1.28587913910472E-16));
#6835=CARTESIAN_POINT('Origin',(0.,1.,0.));
#6836=CARTESIAN_POINT('Origin',(0.,0.,0.));
#6837=CARTESIAN_POINT('',(-1.05,-1.,-1.28587913910472E-16));
#6838=CARTESIAN_POINT('Origin',(0.,-1.,0.));
#6839=CARTESIAN_POINT('',(-1.05,0.,-1.28587913910472E-16));
#6840=CARTESIAN_POINT('Origin',(1.,-1.,0.));
#6841=CARTESIAN_POINT('',(-1.,-1.,-1.22464679914735E-16));
#6842=CARTESIAN_POINT('Origin',(0.,-1.,0.));
#6843=CARTESIAN_POINT('Origin',(0.,-1.065,0.));
#6844=CARTESIAN_POINT('',(-1.,-1.13,-1.22464679914735E-16));
#6845=CARTESIAN_POINT('Origin',(0.,-1.13,0.));
#6846=CARTESIAN_POINT('',(-1.,-1.065,-1.22464679914735E-16));
#6847=CARTESIAN_POINT('Origin',(1.05,-1.13,0.));
#6848=CARTESIAN_POINT('',(-1.05,-1.13,-1.28587913910472E-16));
#6849=CARTESIAN_POINT('Origin',(0.,-1.13,0.));
#6850=CARTESIAN_POINT('Origin',(0.,-1.315,0.));
#6851=CARTESIAN_POINT('',(-1.05,-1.5,-1.28587913910472E-16));
#6852=CARTESIAN_POINT('Origin',(0.,-1.5,0.));
#6853=CARTESIAN_POINT('',(-1.05,-1.315,-1.28587913910472E-16));
#6854=CARTESIAN_POINT('Origin',(0.9,-1.5,0.));
#6855=CARTESIAN_POINT('',(-0.9,-1.5,-1.10218211923262E-16));
#6856=CARTESIAN_POINT('Origin',(0.,-1.5,0.));
#6857=CARTESIAN_POINT('Origin',(0.,0.,0.));
#6858=CARTESIAN_POINT('',(-0.9,0.,-1.10218211923262E-16));
#6859=CARTESIAN_POINT('',(0.,0.,0.));
#6860=CARTESIAN_POINT('Origin',(0.75,1.2,0.));
#6861=CARTESIAN_POINT('',(0.880582193778639,1.2,0.16));
#6862=CARTESIAN_POINT('',(0.880582193778639,1.2,-0.16));
#6863=CARTESIAN_POINT('Origin',(0.,1.2,0.));
#6864=CARTESIAN_POINT('',(0.583459510163302,1.2,0.16));
#6865=CARTESIAN_POINT('',(0.57,1.2,0.16));
#6866=CARTESIAN_POINT('',(0.583459510163302,1.2,-0.16));
#6867=CARTESIAN_POINT('Origin',(0.,1.2,0.));
#6868=CARTESIAN_POINT('',(0.93,1.2,-0.16));
#6869=CARTESIAN_POINT('Origin',(0.93,0.,-0.16));
#6870=CARTESIAN_POINT('',(0.880582193778639,-1.2,-0.16));
#6871=CARTESIAN_POINT('',(0.880582193778639,0.,-0.16));
#6872=CARTESIAN_POINT('',(0.583459510163302,-1.2,-0.16));
#6873=CARTESIAN_POINT('',(0.583459510163302,0.,-0.16));
#6874=CARTESIAN_POINT('',(0.93,-1.2,-0.16));
#6875=CARTESIAN_POINT('Origin',(0.75,-1.2,0.));
#6876=CARTESIAN_POINT('',(0.880582193778639,-1.2,0.16));
#6877=CARTESIAN_POINT('Origin',(0.,-1.2,0.));
#6878=CARTESIAN_POINT('',(0.583459510163302,-1.2,0.16));
#6879=CARTESIAN_POINT('Origin',(0.,-1.2,0.));
#6880=CARTESIAN_POINT('',(0.57,-1.2,0.16));
#6881=CARTESIAN_POINT('Origin',(0.57,0.,0.16));
#6882=CARTESIAN_POINT('',(0.880582193778639,0.,0.16));
#6883=CARTESIAN_POINT('',(0.583459510163302,0.,0.16));
#6884=CARTESIAN_POINT('Origin',(0.895,1.35,0.));
#6885=CARTESIAN_POINT('',(-0.895,1.35,-1.09605888523688E-16));
#6886=CARTESIAN_POINT('Origin',(0.,1.35,0.));
#6887=CARTESIAN_POINT('',(-0.605,1.35,-7.40911313484149E-17));
#6888=CARTESIAN_POINT('Origin',(0.,1.35,0.));
#6889=CARTESIAN_POINT('Origin',(0.,0.,0.));
#6890=CARTESIAN_POINT('',(-0.895,-1.35,-1.09605888523688E-16));
#6891=CARTESIAN_POINT('Origin',(0.,-1.35,0.));
#6892=CARTESIAN_POINT('',(-0.895,0.,-1.09605888523688E-16));
#6893=CARTESIAN_POINT('Origin',(0.605,-1.35,0.));
#6894=CARTESIAN_POINT('',(-0.605,-1.35,-7.40911313484149E-17));
#6895=CARTESIAN_POINT('Origin',(0.,-1.35,0.));
#6896=CARTESIAN_POINT('Origin',(0.,0.,0.));
#6897=CARTESIAN_POINT('',(-0.605,0.,-7.40911313484149E-17));
#6898=CARTESIAN_POINT('',(0.,0.,0.));
#6899=CARTESIAN_POINT('',(0.,0.,0.));
#6900=CARTESIAN_POINT('',(0.,0.,0.));
#6901=CARTESIAN_POINT('',(0.,0.,0.));
#6902=CARTESIAN_POINT('Origin',(-17.3,0.,4.09));
#6903=CARTESIAN_POINT('',(-17.4617868968736,-0.133884278389959,4.09));
#6904=CARTESIAN_POINT('',(-17.1382131031264,-0.133884278389959,4.09));
#6905=CARTESIAN_POINT('',(-17.7,-0.133884278389959,4.09));
#6906=CARTESIAN_POINT('Origin',(-17.3,0.,4.09));
#6907=CARTESIAN_POINT('Origin',(-17.3,0.,4.09));
#6908=CARTESIAN_POINT('',(-17.4617868968736,0.133884278389959,4.09));
#6909=CARTESIAN_POINT('',(-17.51,7.73468293597467E-17,4.105));
#6910=CARTESIAN_POINT('Ctrl Pts',(-17.4617868968736,0.133884278389958,4.09));
#6911=CARTESIAN_POINT('Ctrl Pts',(-17.4747211682176,0.118254395260802,4.09354677224418));
#6912=CARTESIAN_POINT('Ctrl Pts',(-17.4857993165874,0.100109787682302,4.09698224789957));
#6913=CARTESIAN_POINT('Ctrl Pts',(-17.5046385610544,0.0548298721325208,
4.1030741628997));
#6914=CARTESIAN_POINT('Ctrl Pts',(-17.51,0.0266020595922901,4.105));
#6915=CARTESIAN_POINT('Ctrl Pts',(-17.51,-1.73472347597681E-16,4.105));
#6916=CARTESIAN_POINT('',(-17.1382131031264,0.133884278389959,4.09));
#6917=CARTESIAN_POINT('Origin',(-17.3,0.,4.09));
#6918=CARTESIAN_POINT('',(-17.09,-2.66372248183466E-17,4.105));
#6919=CARTESIAN_POINT('Ctrl Pts',(-17.09,1.04083408558608E-16,4.105));
#6920=CARTESIAN_POINT('Ctrl Pts',(-17.09,0.0266020595922904,4.105));
#6921=CARTESIAN_POINT('Ctrl Pts',(-17.0953614389456,0.0548298721325207,
4.1030741628997));
#6922=CARTESIAN_POINT('Ctrl Pts',(-17.1142006834126,0.100109787682302,4.09698224789957));
#6923=CARTESIAN_POINT('Ctrl Pts',(-17.1252788317824,0.118254395260807,4.09354677224418));
#6924=CARTESIAN_POINT('Ctrl Pts',(-17.1382131031264,0.133884278389958,4.09));
#6925=CARTESIAN_POINT('Ctrl Pts',(-17.1382131031264,-0.13388427838996,4.09));
#6926=CARTESIAN_POINT('Ctrl Pts',(-17.1252788317824,-0.118254395260808,
4.09354677224418));
#6927=CARTESIAN_POINT('Ctrl Pts',(-17.1142006834126,-0.100109787682302,
4.09698224789957));
#6928=CARTESIAN_POINT('Ctrl Pts',(-17.0953614389456,-0.0548298721325207,
4.1030741628997));
#6929=CARTESIAN_POINT('Ctrl Pts',(-17.09,-0.0266020595922903,4.105));
#6930=CARTESIAN_POINT('Ctrl Pts',(-17.09,-4.16333634234434E-17,4.105));
#6931=CARTESIAN_POINT('Ctrl Pts',(-17.51,1.87350135405495E-16,4.105));
#6932=CARTESIAN_POINT('Ctrl Pts',(-17.51,-0.0266020595922901,4.105));
#6933=CARTESIAN_POINT('Ctrl Pts',(-17.5046385610544,-0.0548298721325207,
4.1030741628997));
#6934=CARTESIAN_POINT('Ctrl Pts',(-17.4857993165874,-0.100109787682302,
4.09698224789957));
#6935=CARTESIAN_POINT('Ctrl Pts',(-17.4747211682176,-0.118254395260802,
4.09354677224418));
#6936=CARTESIAN_POINT('Ctrl Pts',(-17.4617868968736,-0.133884278389957,
4.09));
#6937=CARTESIAN_POINT('',(-17.51,-2.57175827820945E-17,4.6));
#6938=CARTESIAN_POINT('',(-17.51,-2.57175827820945E-17,4.09));
#6939=CARTESIAN_POINT('',(-17.3,-0.210000000000001,4.57976849370594));
#6940=CARTESIAN_POINT('Ctrl Pts',(-17.3,-0.210000000000001,4.57976849370594));
#6941=CARTESIAN_POINT('Ctrl Pts',(-17.3264385881305,-0.21,4.57976849370594));
#6942=CARTESIAN_POINT('Ctrl Pts',(-17.3545937812549,-0.204702922670978,
4.58084015664674));
#6943=CARTESIAN_POINT('Ctrl Pts',(-17.4063134455413,-0.183251796806355,
4.58468313707126));
#6944=CARTESIAN_POINT('Ctrl Pts',(-17.4298836707411,-0.167101177357215,
4.58739593054622));
#6945=CARTESIAN_POINT('Ctrl Pts',(-17.4671003146174,-0.129884533480966,
4.59246633289124));
#6946=CARTESIAN_POINT('Ctrl Pts',(-17.4832516101634,-0.106313940757288,
4.59515738895358));
#6947=CARTESIAN_POINT('Ctrl Pts',(-17.5047032265697,-0.0545930033295209,
4.59895039220591));
#6948=CARTESIAN_POINT('Ctrl Pts',(-17.51,-0.0264373623835352,4.6));
#6949=CARTESIAN_POINT('Ctrl Pts',(-17.51,6.24500451351651E-17,4.6));
#6950=CARTESIAN_POINT('',(-17.09,-5.00083391933364E-17,4.6));
#6951=CARTESIAN_POINT('Ctrl Pts',(-17.09,3.46944695195361E-17,4.6));
#6952=CARTESIAN_POINT('Ctrl Pts',(-17.09,-0.0264373623835353,4.6));
#6953=CARTESIAN_POINT('Ctrl Pts',(-17.0952967734303,-0.0545930033295208,
4.59895039220591));
#6954=CARTESIAN_POINT('Ctrl Pts',(-17.1167483898366,-0.106313940757288,
4.59515738895358));
#6955=CARTESIAN_POINT('Ctrl Pts',(-17.1328996853826,-0.129884533480966,
4.59246633289124));
#6956=CARTESIAN_POINT('Ctrl Pts',(-17.1701163292589,-0.167101177357215,
4.58739593054622));
#6957=CARTESIAN_POINT('Ctrl Pts',(-17.1936865544587,-0.183251796806355,
4.58468313707126));
#6958=CARTESIAN_POINT('Ctrl Pts',(-17.2454062187451,-0.204702922670978,
4.58084015664674));
#6959=CARTESIAN_POINT('Ctrl Pts',(-17.2735614118695,-0.210000000000001,
4.57976849370594));
#6960=CARTESIAN_POINT('Ctrl Pts',(-17.3,-0.210000000000001,4.57976849370594));
#6961=CARTESIAN_POINT('Ctrl Pts',(-17.51,-9.71445146547012E-17,4.6));
#6962=CARTESIAN_POINT('Ctrl Pts',(-17.51,0.0264373623835352,4.6));
#6963=CARTESIAN_POINT('Ctrl Pts',(-17.5047032265697,0.0545930033295208,
4.59895039220591));
#6964=CARTESIAN_POINT('Ctrl Pts',(-17.4832516101634,0.106313940757288,4.59515738895358));
#6965=CARTESIAN_POINT('Ctrl Pts',(-17.4671003146174,0.129884533480966,4.59246633289124));
#6966=CARTESIAN_POINT('Ctrl Pts',(-17.4298836707411,0.167101177357215,4.58739593054622));
#6967=CARTESIAN_POINT('Ctrl Pts',(-17.4063134455413,0.183251796806355,4.58468313707126));
#6968=CARTESIAN_POINT('Ctrl Pts',(-17.3545937812549,0.204702922670978,4.58084015664674));
#6969=CARTESIAN_POINT('Ctrl Pts',(-17.3264385881305,0.210000000000001,4.57976849370594));
#6970=CARTESIAN_POINT('Ctrl Pts',(-17.2735614118695,0.210000000000001,4.57976849370594));
#6971=CARTESIAN_POINT('Ctrl Pts',(-17.2454062187451,0.204702922670978,4.58084015664674));
#6972=CARTESIAN_POINT('Ctrl Pts',(-17.1936865544587,0.183251796806355,4.58468313707126));
#6973=CARTESIAN_POINT('Ctrl Pts',(-17.1701163292589,0.167101177357215,4.58739593054622));
#6974=CARTESIAN_POINT('Ctrl Pts',(-17.1328996853826,0.129884533480966,4.59246633289124));
#6975=CARTESIAN_POINT('Ctrl Pts',(-17.1167483898366,0.106313940757288,4.59515738895358));
#6976=CARTESIAN_POINT('Ctrl Pts',(-17.0952967734303,0.0545930033295209,
4.59895039220591));
#6977=CARTESIAN_POINT('Ctrl Pts',(-17.09,0.0264373623835352,4.6));
#6978=CARTESIAN_POINT('Ctrl Pts',(-17.09,-1.11022302462516E-16,4.6));
#6979=CARTESIAN_POINT('Origin',(-17.3,0.,4.09));
#6980=CARTESIAN_POINT('',(-17.7,0.133884278389959,4.09));
#6981=CARTESIAN_POINT('Origin',(-17.7,0.,3.5));
#6982=CARTESIAN_POINT('',(-16.9,-7.40911313484149E-17,4.105));
#6983=CARTESIAN_POINT('Origin',(-16.9,0.,3.5));
#6984=CARTESIAN_POINT('',(-17.7,-7.40911313484149E-17,4.105));
#6985=CARTESIAN_POINT('',(-17.7,-7.40911313484149E-17,4.105));
#6986=CARTESIAN_POINT('',(-17.7,-7.40911313484149E-17,4.105));
#6987=CARTESIAN_POINT('Origin',(-17.7,0.,3.5));
#6988=CARTESIAN_POINT('Origin',(-17.7,0.,3.5));
#6989=CARTESIAN_POINT('',(-16.9,-1.34711147906209E-16,4.6));
#6990=CARTESIAN_POINT('Origin',(-16.9,0.,3.5));
#6991=CARTESIAN_POINT('',(-17.7,-1.34711147906209E-16,4.6));
#6992=CARTESIAN_POINT('',(-17.7,-1.34711147906209E-16,4.6));
#6993=CARTESIAN_POINT('',(-17.7,-1.34711147906209E-16,4.6));
#6994=CARTESIAN_POINT('Origin',(-17.7,0.,3.5));
#6995=CARTESIAN_POINT('Origin',(-16.9,0.,3.5));
#6996=CARTESIAN_POINT('Origin',(-17.7,0.,3.5));
#6997=CARTESIAN_POINT('',(0.,0.,0.));
#6998=CARTESIAN_POINT('Origin',(11.9,0.,4.09));
#6999=CARTESIAN_POINT('',(11.7382131031264,-0.133884278389959,4.09));
#7000=CARTESIAN_POINT('',(12.0617868968736,-0.133884278389959,4.09));
#7001=CARTESIAN_POINT('',(11.5,-0.133884278389959,4.09));
#7002=CARTESIAN_POINT('Origin',(11.9,0.,4.09));
#7003=CARTESIAN_POINT('Origin',(11.9,0.,4.09));
#7004=CARTESIAN_POINT('',(11.7382131031264,0.133884278389959,4.09));
#7005=CARTESIAN_POINT('',(11.69,-3.02060261508153E-17,4.105));
#7006=CARTESIAN_POINT('Ctrl Pts',(11.7382131031264,0.13388427838996,4.09));
#7007=CARTESIAN_POINT('Ctrl Pts',(11.7252788317824,0.118254395260805,4.09354677224418));
#7008=CARTESIAN_POINT('Ctrl Pts',(11.7142006834126,0.100109787682301,4.09698224789957));
#7009=CARTESIAN_POINT('Ctrl Pts',(11.6953614389456,0.0548298721325195,4.1030741628997));
#7010=CARTESIAN_POINT('Ctrl Pts',(11.69,0.0266020595922904,4.105));
#7011=CARTESIAN_POINT('Ctrl Pts',(11.69,0.,4.105));
#7012=CARTESIAN_POINT('',(12.0617868968736,0.133884278389959,4.09));
#7013=CARTESIAN_POINT('Origin',(11.9,0.,4.09));
#7014=CARTESIAN_POINT('',(12.11,-8.21483760496044E-17,4.105));
#7015=CARTESIAN_POINT('Ctrl Pts',(12.11,-1.45716771982052E-16,4.105));
#7016=CARTESIAN_POINT('Ctrl Pts',(12.11,0.0266020595922903,4.105));
#7017=CARTESIAN_POINT('Ctrl Pts',(12.1046385610544,0.0548298721325195,4.1030741628997));
#7018=CARTESIAN_POINT('Ctrl Pts',(12.0857993165874,0.1001097876823,4.09698224789957));
#7019=CARTESIAN_POINT('Ctrl Pts',(12.0747211682176,0.118254395260803,4.09354677224418));
#7020=CARTESIAN_POINT('Ctrl Pts',(12.0617868968736,0.133884278389959,4.09));
#7021=CARTESIAN_POINT('Ctrl Pts',(12.0617868968736,-0.133884278389959,4.09));
#7022=CARTESIAN_POINT('Ctrl Pts',(12.0747211682176,-0.118254395260804,4.09354677224418));
#7023=CARTESIAN_POINT('Ctrl Pts',(12.0857993165874,-0.1001097876823,4.09698224789957));
#7024=CARTESIAN_POINT('Ctrl Pts',(12.1046385610544,-0.0548298721325195,
4.1030741628997));
#7025=CARTESIAN_POINT('Ctrl Pts',(12.11,-0.0266020595922902,4.105));
#7026=CARTESIAN_POINT('Ctrl Pts',(12.11,2.56739074444567E-16,4.105));
#7027=CARTESIAN_POINT('Ctrl Pts',(11.69,7.63278329429795E-17,4.105));
#7028=CARTESIAN_POINT('Ctrl Pts',(11.69,-0.0266020595922903,4.105));
#7029=CARTESIAN_POINT('Ctrl Pts',(11.6953614389456,-0.0548298721325195,
4.1030741628997));
#7030=CARTESIAN_POINT('Ctrl Pts',(11.7142006834126,-0.1001097876823,4.09698224789957));
#7031=CARTESIAN_POINT('Ctrl Pts',(11.7252788317824,-0.118254395260804,4.09354677224418));
#7032=CARTESIAN_POINT('Ctrl Pts',(11.7382131031264,-0.133884278389959,4.09));
#7033=CARTESIAN_POINT('',(11.69,-2.57175827820945E-17,4.6));
#7034=CARTESIAN_POINT('',(11.69,-2.57175827820945E-17,4.09));
#7035=CARTESIAN_POINT('',(11.9,-0.210000000000001,4.57976849370594));
#7036=CARTESIAN_POINT('Ctrl Pts',(11.9,-0.210000000000001,4.57976849370594));
#7037=CARTESIAN_POINT('Ctrl Pts',(11.8735614118695,-0.210000000000001,4.57976849370594));
#7038=CARTESIAN_POINT('Ctrl Pts',(11.8454062187451,-0.204702922670977,4.58084015664674));
#7039=CARTESIAN_POINT('Ctrl Pts',(11.7936865544587,-0.183251796806355,4.58468313707126));
#7040=CARTESIAN_POINT('Ctrl Pts',(11.7701163292589,-0.167101177357215,4.58739593054622));
#7041=CARTESIAN_POINT('Ctrl Pts',(11.7328996853826,-0.129884533480966,4.59246633289124));
#7042=CARTESIAN_POINT('Ctrl Pts',(11.7167483898366,-0.10631394075729,4.59515738895358));
#7043=CARTESIAN_POINT('Ctrl Pts',(11.6952967734303,-0.0545930033295214,
4.59895039220591));
#7044=CARTESIAN_POINT('Ctrl Pts',(11.69,-0.0264373623835355,4.6));
#7045=CARTESIAN_POINT('Ctrl Pts',(11.69,-3.12250225675825E-17,4.6));
#7046=CARTESIAN_POINT('',(12.11,2.28500467976895E-17,4.6));
#7047=CARTESIAN_POINT('Ctrl Pts',(12.11,1.52655665885959E-16,4.6));
#7048=CARTESIAN_POINT('Ctrl Pts',(12.11,-0.0264373623835353,4.6));
#7049=CARTESIAN_POINT('Ctrl Pts',(12.1047032265697,-0.0545930033295213,
4.59895039220591));
#7050=CARTESIAN_POINT('Ctrl Pts',(12.0832516101634,-0.106313940757289,4.59515738895358));
#7051=CARTESIAN_POINT('Ctrl Pts',(12.0671003146174,-0.129884533480966,4.59246633289124));
#7052=CARTESIAN_POINT('Ctrl Pts',(12.0298836707411,-0.167101177357215,4.58739593054622));
#7053=CARTESIAN_POINT('Ctrl Pts',(12.0063134455413,-0.183251796806355,4.58468313707126));
#7054=CARTESIAN_POINT('Ctrl Pts',(11.9545937812549,-0.204702922670977,4.58084015664674));
#7055=CARTESIAN_POINT('Ctrl Pts',(11.9264385881305,-0.210000000000001,4.57976849370594));
#7056=CARTESIAN_POINT('Ctrl Pts',(11.9,-0.210000000000001,4.57976849370594));
#7057=CARTESIAN_POINT('Ctrl Pts',(11.69,6.59194920871187E-17,4.6));
#7058=CARTESIAN_POINT('Ctrl Pts',(11.69,0.0264373623835355,4.6));
#7059=CARTESIAN_POINT('Ctrl Pts',(11.6952967734303,0.0545930033295213,4.59895039220591));
#7060=CARTESIAN_POINT('Ctrl Pts',(11.7167483898366,0.106313940757289,4.59515738895358));
#7061=CARTESIAN_POINT('Ctrl Pts',(11.7328996853826,0.129884533480966,4.59246633289124));
#7062=CARTESIAN_POINT('Ctrl Pts',(11.7701163292589,0.167101177357215,4.58739593054622));
#7063=CARTESIAN_POINT('Ctrl Pts',(11.7936865544587,0.183251796806355,4.58468313707126));
#7064=CARTESIAN_POINT('Ctrl Pts',(11.8454062187451,0.204702922670977,4.58084015664674));
#7065=CARTESIAN_POINT('Ctrl Pts',(11.8735614118695,0.210000000000001,4.57976849370594));
#7066=CARTESIAN_POINT('Ctrl Pts',(11.9264385881305,0.210000000000001,4.57976849370594));
#7067=CARTESIAN_POINT('Ctrl Pts',(11.9545937812549,0.204702922670977,4.58084015664674));
#7068=CARTESIAN_POINT('Ctrl Pts',(12.0063134455413,0.183251796806355,4.58468313707126));
#7069=CARTESIAN_POINT('Ctrl Pts',(12.0298836707411,0.167101177357215,4.58739593054622));
#7070=CARTESIAN_POINT('Ctrl Pts',(12.0671003146174,0.129884533480966,4.59246633289124));
#7071=CARTESIAN_POINT('Ctrl Pts',(12.0832516101634,0.106313940757289,4.59515738895358));
#7072=CARTESIAN_POINT('Ctrl Pts',(12.1047032265697,0.0545930033295214,4.59895039220591));
#7073=CARTESIAN_POINT('Ctrl Pts',(12.11,0.0264373623835354,4.6));
#7074=CARTESIAN_POINT('Ctrl Pts',(12.11,-4.16333634234434E-17,4.6));
#7075=CARTESIAN_POINT('Origin',(11.9,0.,4.09));
#7076=CARTESIAN_POINT('',(11.5,0.133884278389959,4.09));
#7077=CARTESIAN_POINT('Origin',(11.5,0.,3.5));
#7078=CARTESIAN_POINT('',(12.3,-7.40911313484149E-17,4.105));
#7079=CARTESIAN_POINT('Origin',(12.3,0.,3.5));
#7080=CARTESIAN_POINT('',(11.5,-7.40911313484149E-17,4.105));
#7081=CARTESIAN_POINT('',(11.5,-7.40911313484149E-17,4.105));
#7082=CARTESIAN_POINT('',(11.5,-7.40911313484149E-17,4.105));
#7083=CARTESIAN_POINT('Origin',(11.5,0.,3.5));
#7084=CARTESIAN_POINT('Origin',(11.5,0.,3.5));
#7085=CARTESIAN_POINT('',(12.3,-1.34711147906209E-16,4.6));
#7086=CARTESIAN_POINT('Origin',(12.3,0.,3.5));
#7087=CARTESIAN_POINT('',(11.5,-1.34711147906209E-16,4.6));
#7088=CARTESIAN_POINT('',(11.5,-1.34711147906209E-16,4.6));
#7089=CARTESIAN_POINT('',(11.5,-1.34711147906209E-16,4.6));
#7090=CARTESIAN_POINT('Origin',(11.5,0.,3.5));
#7091=CARTESIAN_POINT('Origin',(12.3,0.,3.5));
#7092=CARTESIAN_POINT('Origin',(11.5,0.,3.5));
#7093=CARTESIAN_POINT('',(0.,0.,0.));
#7094=CARTESIAN_POINT('Origin',(12.5,0.,3.5));
#7095=CARTESIAN_POINT('',(12.5,-4.59242549680257E-17,3.875));
#7096=CARTESIAN_POINT('Origin',(12.5,0.,3.5));
#7097=CARTESIAN_POINT('',(12.8,4.59242549680257E-17,3.875));
#7098=CARTESIAN_POINT('',(12.5,-4.59242549680257E-17,3.875));
#7099=CARTESIAN_POINT('Origin',(12.8,0.,3.5));
#7100=CARTESIAN_POINT('Origin',(12.5,0.,3.5));
#7101=CARTESIAN_POINT('',(12.5,-2.75545529808155E-17,3.725));
#7102=CARTESIAN_POINT('Origin',(12.5,0.,3.5));
#7103=CARTESIAN_POINT('Origin',(12.3,0.,3.5));
#7104=CARTESIAN_POINT('',(12.3,-2.75545529808155E-17,3.725));
#7105=CARTESIAN_POINT('',(12.3,-2.75545529808155E-17,3.725));
#7106=CARTESIAN_POINT('Origin',(12.3,0.,3.5));
#7107=CARTESIAN_POINT('Origin',(12.3,0.,3.5));
#7108=CARTESIAN_POINT('',(12.8,-1.71450551880629E-16,4.9));
#7109=CARTESIAN_POINT('Origin',(12.8,0.,3.5));
#7110=CARTESIAN_POINT('',(12.3,-1.71450551880629E-16,4.9));
#7111=CARTESIAN_POINT('',(12.3,-1.71450551880629E-16,4.9));
#7112=CARTESIAN_POINT('Origin',(12.3,0.,3.5));
#7113=CARTESIAN_POINT('Origin',(12.8,0.,3.5));
#7114=CARTESIAN_POINT('Origin',(12.3,0.,3.5));
#7115=CARTESIAN_POINT('',(0.,0.,0.));
#7116=CARTESIAN_POINT('Origin',(28.5,0.,0.));
#7117=CARTESIAN_POINT('',(28.5,-2.02066721859313E-17,0.165));
#7118=CARTESIAN_POINT('Origin',(28.5,0.,0.));
#7119=CARTESIAN_POINT('',(30.,2.02066721859313E-17,0.165));
#7120=CARTESIAN_POINT('',(28.5,-2.02066721859313E-17,0.165));
#7121=CARTESIAN_POINT('Origin',(30.,0.,0.));
#7122=CARTESIAN_POINT('Origin',(28.5,0.,0.));
#7123=CARTESIAN_POINT('Origin',(0.05,0.,0.));
#7124=CARTESIAN_POINT('',(0.1,7.34788079488412E-17,0.6));
#7125=CARTESIAN_POINT('Origin',(0.1,0.,0.));
#7126=CARTESIAN_POINT('',(0.,-6.12323399573677E-17,0.5));
#7127=CARTESIAN_POINT('',(0.05,-6.73555739531044E-17,0.55));
#7128=CARTESIAN_POINT('Origin',(0.,0.,0.));
#7129=CARTESIAN_POINT('Origin',(0.,0.,0.));
#7130=CARTESIAN_POINT('',(29.9,-7.34788079488412E-17,0.6));
#7131=CARTESIAN_POINT('Origin',(29.9,0.,0.));
#7132=CARTESIAN_POINT('',(0.,-7.34788079488412E-17,0.6));
#7133=CARTESIAN_POINT('Origin',(0.,0.,0.));
#7134=CARTESIAN_POINT('Origin',(29.95,0.,0.));
#7135=CARTESIAN_POINT('',(30.,6.12323399573677E-17,0.5));
#7136=CARTESIAN_POINT('Origin',(30.,0.,0.));
#7137=CARTESIAN_POINT('',(29.95,-6.73555739531044E-17,0.55));
#7138=CARTESIAN_POINT('Origin',(30.,0.,0.));
#7139=CARTESIAN_POINT('',(0.,0.,0.));
#7140=CARTESIAN_POINT('Origin',(0.0721687836487032,0.,-0.125));
#7141=CARTESIAN_POINT('',(0.0721687836487032,0.,-0.125));
#7142=CARTESIAN_POINT('',(0.144337567297406,0.,0.));
#7143=CARTESIAN_POINT('',(0.117710979560879,0.,-0.0461186027918559));
#7144=CARTESIAN_POINT('',(0.0721687836487032,-0.25,-0.125));
#7145=CARTESIAN_POINT('',(0.0721687836487032,0.,-0.125));
#7146=CARTESIAN_POINT('',(0.144337567297406,-0.25,0.));
#7147=CARTESIAN_POINT('',(0.144337567297406,-0.25,0.));
#7148=CARTESIAN_POINT('',(0.144337567297406,0.,0.));
#7149=CARTESIAN_POINT('Origin',(-0.0721687836487032,0.,-0.125));
#7150=CARTESIAN_POINT('',(-0.0721687836487032,0.,-0.125));
#7151=CARTESIAN_POINT('',(0.0739156081756484,0.,-0.125));
#7152=CARTESIAN_POINT('',(-0.0721687836487032,-0.25,-0.125));
#7153=CARTESIAN_POINT('',(-0.0721687836487032,0.,-0.125));
#7154=CARTESIAN_POINT('',(0.0721687836487032,-0.25,-0.125));
#7155=CARTESIAN_POINT('Origin',(-0.144337567297406,0.,-4.16333634234434E-17));
#7156=CARTESIAN_POINT('',(-0.144337567297406,0.,-1.76762539787485E-17));
#7157=CARTESIAN_POINT('',(-0.0987953713852306,0.,-0.0788813972081442));
#7158=CARTESIAN_POINT('',(-0.144337567297406,-0.25,-2.77555756156289E-17));
#7159=CARTESIAN_POINT('',(-0.144337567297406,0.,-1.76762539787485E-17));
#7160=CARTESIAN_POINT('',(-0.0721687836487032,-0.25,-0.125));
#7161=CARTESIAN_POINT('Origin',(-0.0721687836487033,0.,0.125));
#7162=CARTESIAN_POINT('',(-0.0721687836487033,0.,0.125));
#7163=CARTESIAN_POINT('',(-0.0627109795608791,0.,0.141381397208144));
#7164=CARTESIAN_POINT('',(-0.0721687836487033,-0.25,0.125));
#7165=CARTESIAN_POINT('',(-0.0721687836487033,0.,0.125));
#7166=CARTESIAN_POINT('',(-0.144337567297406,-0.25,-1.76762539787485E-17));
#7167=CARTESIAN_POINT('Origin',(0.0721687836487032,0.,0.125));
#7168=CARTESIAN_POINT('',(0.0721687836487032,0.,0.125));
#7169=CARTESIAN_POINT('',(0.146084391824352,0.,0.125));
#7170=CARTESIAN_POINT('',(0.0721687836487032,-0.25,0.125));
#7171=CARTESIAN_POINT('',(0.0721687836487032,0.,0.125));
#7172=CARTESIAN_POINT('',(-0.0721687836487033,-0.25,0.125));
#7173=CARTESIAN_POINT('Origin',(0.144337567297406,0.,0.));
#7174=CARTESIAN_POINT('',(0.153795371385231,0.,-0.0163813972081441));
#7175=CARTESIAN_POINT('',(0.0721687836487032,-0.25,0.125));
#7176=CARTESIAN_POINT('Origin',(0.,-0.25,0.));
#7177=CARTESIAN_POINT('Origin',(0.22,0.,0.));
#7178=CARTESIAN_POINT('',(-0.22,-8.67361737988404E-18,-2.69422295812418E-17));
#7179=CARTESIAN_POINT('Origin',(0.,0.,0.));
#7180=CARTESIAN_POINT('Origin',(0.,-0.015,0.));
#7181=CARTESIAN_POINT('',(-0.24505,-0.02505,-3.00099698131059E-17));
#7182=CARTESIAN_POINT('Origin',(0.,-0.02505,0.));
#7183=CARTESIAN_POINT('',(-0.235,-0.015,-2.87791997799628E-17));
#7184=CARTESIAN_POINT('Origin',(0.,-0.3775,0.));
#7185=CARTESIAN_POINT('',(-0.24505,-0.72995,3.00099698131059E-17));
#7186=CARTESIAN_POINT('Origin',(0.,-0.72995,0.));
#7187=CARTESIAN_POINT('',(-0.24505,-0.3775,-3.00099698131059E-17));
#7188=CARTESIAN_POINT('Origin',(0.,-0.7625,0.));
#7189=CARTESIAN_POINT('',(-0.175,-0.8,-2.14313189850787E-17));
#7190=CARTESIAN_POINT('Origin',(0.,-0.8,0.));
#7191=CARTESIAN_POINT('',(-0.2125,-0.7625,-2.60237444818813E-17));
#7192=CARTESIAN_POINT('Origin',(0.,-0.8,0.));
#7193=CARTESIAN_POINT('',(0.,0.,0.));
#7194=CARTESIAN_POINT('Origin',(0.3,0.4,0.));
#7195=CARTESIAN_POINT('',(-0.3,0.4,-3.67394039744206E-17));
#7196=CARTESIAN_POINT('Origin',(0.,0.4,0.));
#7197=CARTESIAN_POINT('Origin',(0.,0.375,0.));
#7198=CARTESIAN_POINT('',(-0.35,0.35,-4.28626379701573E-17));
#7199=CARTESIAN_POINT('Origin',(0.,0.35,0.));
#7200=CARTESIAN_POINT('',(-0.325,0.375,-3.9801020972289E-17));
#7201=CARTESIAN_POINT('Origin',(0.,0.19,0.));
#7202=CARTESIAN_POINT('',(-0.35,0.03,-4.28626379701574E-17));
#7203=CARTESIAN_POINT('Origin',(0.,0.03,0.));
#7204=CARTESIAN_POINT('',(-0.35,0.19,-4.28626379701574E-17));
#7205=CARTESIAN_POINT('Origin',(0.,0.0149999999999999,0.));
#7206=CARTESIAN_POINT('',(-0.32,-3.29597460435593E-17,-3.91886975727153E-17));
#7207=CARTESIAN_POINT('Origin',(0.,0.,0.));
#7208=CARTESIAN_POINT('',(-0.335,0.0149999999999999,-4.10256677714363E-17));
#7209=CARTESIAN_POINT('Origin',(0.22,0.,0.));
#7210=CARTESIAN_POINT('',(-0.22,-6.93889390390723E-18,-2.69422295812418E-17));
#7211=CARTESIAN_POINT('Origin',(0.,0.,0.));
#7212=CARTESIAN_POINT('Origin',(0.,-0.02,0.));
#7213=CARTESIAN_POINT('',(-0.1954,-0.0492,2.39295984553393E-17));
#7214=CARTESIAN_POINT('Origin',(0.,-0.0492,0.));
#7215=CARTESIAN_POINT('',(-0.21,-0.02,-2.57175827820944E-17));
#7216=CARTESIAN_POINT('Origin',(0.,-0.8,0.));
#7217=CARTESIAN_POINT('',(-0.1954,-1.5646,2.39295984553393E-17));
#7218=CARTESIAN_POINT('Origin',(0.,-1.5646,0.));
#7219=CARTESIAN_POINT('',(-0.1954,-0.8,-2.39295984553393E-17));
#7220=CARTESIAN_POINT('Origin',(0.,-1.58,0.));
#7221=CARTESIAN_POINT('',(-0.16,-1.6,-1.95943487863577E-17));
#7222=CARTESIAN_POINT('Origin',(0.,-1.6,0.));
#7223=CARTESIAN_POINT('',(-0.18,-1.58,-2.20436423846524E-17));
#7224=CARTESIAN_POINT('Origin',(0.,-1.6,0.));
#7225=CARTESIAN_POINT('Origin',(0.0866025403784439,-0.4,-0.15));
#7226=CARTESIAN_POINT('',(0.173205080756888,-0.4,0.));
#7227=CARTESIAN_POINT('',(0.0866025403784439,-0.4,-0.15));
#7228=CARTESIAN_POINT('',(0.173205080756888,-0.4,0.));
#7229=CARTESIAN_POINT('',(0.0866025403784439,-0.64,-0.15));
#7230=CARTESIAN_POINT('',(0.0866025403784439,-0.4,-0.15));
#7231=CARTESIAN_POINT('',(0.173205080756888,-0.64,0.));
#7232=CARTESIAN_POINT('',(0.173205080756888,-0.64,0.));
#7233=CARTESIAN_POINT('',(0.173205080756888,-0.4,0.));
#7234=CARTESIAN_POINT('Origin',(-0.0866025403784438,-0.4,-0.15));
#7235=CARTESIAN_POINT('',(-0.0866025403784438,-0.4,-0.15));
#7236=CARTESIAN_POINT('',(0.0866025403784439,-0.4,-0.15));
#7237=CARTESIAN_POINT('',(-0.0866025403784438,-0.64,-0.15));
#7238=CARTESIAN_POINT('',(-0.0866025403784438,-0.4,-0.15));
#7239=CARTESIAN_POINT('',(0.0866025403784439,-0.64,-0.15));
#7240=CARTESIAN_POINT('Origin',(-0.173205080756888,-0.4,-2.77555756156289E-17));
#7241=CARTESIAN_POINT('',(-0.173205080756888,-0.4,-2.12115047744981E-17));
#7242=CARTESIAN_POINT('',(-0.0866025403784438,-0.4,-0.15));
#7243=CARTESIAN_POINT('',(-0.173205080756888,-0.64,-2.77555756156289E-17));
#7244=CARTESIAN_POINT('',(-0.173205080756888,-0.4,-2.12115047744981E-17));
#7245=CARTESIAN_POINT('',(-0.0866025403784438,-0.64,-0.15));
#7246=CARTESIAN_POINT('Origin',(-0.0866025403784439,-0.4,0.15));
#7247=CARTESIAN_POINT('',(-0.0866025403784439,-0.4,0.15));
#7248=CARTESIAN_POINT('',(-0.173205080756888,-0.4,-2.12115047744981E-17));
#7249=CARTESIAN_POINT('',(-0.0866025403784439,-0.64,0.15));
#7250=CARTESIAN_POINT('',(-0.0866025403784439,-0.4,0.15));
#7251=CARTESIAN_POINT('',(-0.173205080756888,-0.64,-2.12115047744981E-17));
#7252=CARTESIAN_POINT('Origin',(0.0866025403784439,-0.4,0.15));
#7253=CARTESIAN_POINT('',(0.0866025403784439,-0.4,0.15));
#7254=CARTESIAN_POINT('',(-0.0866025403784439,-0.4,0.15));
#7255=CARTESIAN_POINT('',(0.0866025403784439,-0.64,0.15));
#7256=CARTESIAN_POINT('',(0.0866025403784439,-0.4,0.15));
#7257=CARTESIAN_POINT('',(-0.0866025403784439,-0.64,0.15));
#7258=CARTESIAN_POINT('Origin',(0.173205080756888,-0.4,0.));
#7259=CARTESIAN_POINT('',(0.0866025403784439,-0.4,0.15));
#7260=CARTESIAN_POINT('',(0.0866025403784439,-0.64,0.15));
#7261=CARTESIAN_POINT('Origin',(0.,-0.4,-2.77555756156289E-17));
#7262=CARTESIAN_POINT('Origin',(0.,-0.64,-2.77555756156289E-17));
#7263=CARTESIAN_POINT('',(0.,0.,0.));
#7264=CARTESIAN_POINT('',(0.,0.,0.));
#7265=CARTESIAN_POINT('',(0.,0.,0.));
#7266=CARTESIAN_POINT('',(0.,0.,0.));
#7267=CARTESIAN_POINT('',(0.,0.,0.));
#7268=CARTESIAN_POINT('',(0.,0.,0.));
#7269=CARTESIAN_POINT('',(0.,0.,0.));
#7270=CARTESIAN_POINT('',(0.,0.,0.));
#7271=CARTESIAN_POINT('',(0.,0.,0.));
#7272=CARTESIAN_POINT('',(0.,0.,0.));
#7273=CARTESIAN_POINT('',(0.,0.,0.));
#7274=CARTESIAN_POINT('',(2.2,-2.1,0.));
#7275=CARTESIAN_POINT('',(2.2,-2.1,4.8));
#7276=CARTESIAN_POINT('',(2.2,2.1,0.));
#7277=CARTESIAN_POINT('',(2.2,2.1,4.8));
#7278=CARTESIAN_POINT('',(7.8,-2.1,0.));
#7279=CARTESIAN_POINT('',(7.8,-2.1,4.8));
#7280=CARTESIAN_POINT('',(7.8,2.1,0.));
#7281=CARTESIAN_POINT('',(7.8,2.1,4.8));
#7282=CARTESIAN_POINT('',(2.5,0.,3.5));
#7283=CARTESIAN_POINT('',(7.5,0.,3.5));
#7284=CARTESIAN_POINT('',(-0.5,1.04094977927525E-16,5.2));
#7285=CARTESIAN_POINT('',(-0.5,-1.47224318643355,2.65));
#7286=CARTESIAN_POINT('',(-0.5,1.47224318643355,2.65));
#7287=CARTESIAN_POINT('',(11.,1.1,4.5));
#7288=CARTESIAN_POINT('',(10.5,1.04094977927525E-16,5.2));
#7289=CARTESIAN_POINT('',(10.5,-1.47224318643355,2.65));
#7290=CARTESIAN_POINT('',(10.5,1.47224318643355,2.65));
#7291=CARTESIAN_POINT('',(0.,0.,0.));
#7292=CARTESIAN_POINT('',(0.,0.,0.));
#7293=CARTESIAN_POINT('',(0.,0.,0.));
#7294=CARTESIAN_POINT('',(-17.7,0.,3.5));
#7295=CARTESIAN_POINT('',(-17.3,0.,4.9));
#7296=CARTESIAN_POINT('',(11.9,0.,4.9));
#7297=CARTESIAN_POINT('',(12.5,-9.86076131526265E-32,3.5));
#7298=CARTESIAN_POINT('',(0.,0.,0.));
#7299=CARTESIAN_POINT('',(0.,0.,0.));
#7300=UNCERTAINTY_MEASURE_WITH_UNIT(LENGTH_MEASURE(0.001),#7350,
'DISTANCE_ACCURACY_VALUE',
'Maximum model space distance between geometric entities at asserted c
onnectivities');
#7301=UNCERTAINTY_MEASURE_WITH_UNIT(LENGTH_MEASURE(0.001),#7350,
'DISTANCE_ACCURACY_VALUE',
'Maximum model space distance between geometric entities at asserted c
onnectivities');
#7302=UNCERTAINTY_MEASURE_WITH_UNIT(LENGTH_MEASURE(0.001),#7350,
'DISTANCE_ACCURACY_VALUE',
'Maximum model space distance between geometric entities at asserted c
onnectivities');
#7303=UNCERTAINTY_MEASURE_WITH_UNIT(LENGTH_MEASURE(0.001),#7350,
'DISTANCE_ACCURACY_VALUE',
'Maximum model space distance between geometric entities at asserted c
onnectivities');
#7304=UNCERTAINTY_MEASURE_WITH_UNIT(LENGTH_MEASURE(0.001),#7350,
'DISTANCE_ACCURACY_VALUE',
'Maximum model space distance between geometric entities at asserted c
onnectivities');
#7305=UNCERTAINTY_MEASURE_WITH_UNIT(LENGTH_MEASURE(0.001),#7350,
'DISTANCE_ACCURACY_VALUE',
'Maximum model space distance between geometric entities at asserted c
onnectivities');
#7306=UNCERTAINTY_MEASURE_WITH_UNIT(LENGTH_MEASURE(0.001),#7350,
'DISTANCE_ACCURACY_VALUE',
'Maximum model space distance between geometric entities at asserted c
onnectivities');
#7307=UNCERTAINTY_MEASURE_WITH_UNIT(LENGTH_MEASURE(0.001),#7350,
'DISTANCE_ACCURACY_VALUE',
'Maximum model space distance between geometric entities at asserted c
onnectivities');
#7308=UNCERTAINTY_MEASURE_WITH_UNIT(LENGTH_MEASURE(0.001),#7350,
'DISTANCE_ACCURACY_VALUE',
'Maximum model space distance between geometric entities at asserted c
onnectivities');
#7309=UNCERTAINTY_MEASURE_WITH_UNIT(LENGTH_MEASURE(0.001),#7350,
'DISTANCE_ACCURACY_VALUE',
'Maximum model space distance between geometric entities at asserted c
onnectivities');
#7310=UNCERTAINTY_MEASURE_WITH_UNIT(LENGTH_MEASURE(0.001),#7350,
'DISTANCE_ACCURACY_VALUE',
'Maximum model space distance between geometric entities at asserted c
onnectivities');
#7311=UNCERTAINTY_MEASURE_WITH_UNIT(LENGTH_MEASURE(0.001),#7350,
'DISTANCE_ACCURACY_VALUE',
'Maximum model space distance between geometric entities at asserted c
onnectivities');
#7312=UNCERTAINTY_MEASURE_WITH_UNIT(LENGTH_MEASURE(0.001),#7350,
'DISTANCE_ACCURACY_VALUE',
'Maximum model space distance between geometric entities at asserted c
onnectivities');
#7313=UNCERTAINTY_MEASURE_WITH_UNIT(LENGTH_MEASURE(0.001),#7350,
'DISTANCE_ACCURACY_VALUE',
'Maximum model space distance between geometric entities at asserted c
onnectivities');
#7314=UNCERTAINTY_MEASURE_WITH_UNIT(LENGTH_MEASURE(0.001),#7350,
'DISTANCE_ACCURACY_VALUE',
'Maximum model space distance between geometric entities at asserted c
onnectivities');
#7315=UNCERTAINTY_MEASURE_WITH_UNIT(LENGTH_MEASURE(0.001),#7350,
'DISTANCE_ACCURACY_VALUE',
'Maximum model space distance between geometric entities at asserted c
onnectivities');
#7316=UNCERTAINTY_MEASURE_WITH_UNIT(LENGTH_MEASURE(0.001),#7350,
'DISTANCE_ACCURACY_VALUE',
'Maximum model space distance between geometric entities at asserted c
onnectivities');
#7317=UNCERTAINTY_MEASURE_WITH_UNIT(LENGTH_MEASURE(0.001),#7350,
'DISTANCE_ACCURACY_VALUE',
'Maximum model space distance between geometric entities at asserted c
onnectivities');
#7318=UNCERTAINTY_MEASURE_WITH_UNIT(LENGTH_MEASURE(0.001),#7350,
'DISTANCE_ACCURACY_VALUE',
'Maximum model space distance between geometric entities at asserted c
onnectivities');
#7319=UNCERTAINTY_MEASURE_WITH_UNIT(LENGTH_MEASURE(0.001),#7350,
'DISTANCE_ACCURACY_VALUE',
'Maximum model space distance between geometric entities at asserted c
onnectivities');
#7320=UNCERTAINTY_MEASURE_WITH_UNIT(LENGTH_MEASURE(0.001),#7350,
'DISTANCE_ACCURACY_VALUE',
'Maximum model space distance between geometric entities at asserted c
onnectivities');
#7321=UNCERTAINTY_MEASURE_WITH_UNIT(LENGTH_MEASURE(0.001),#7350,
'DISTANCE_ACCURACY_VALUE',
'Maximum model space distance between geometric entities at asserted c
onnectivities');
#7322=UNCERTAINTY_MEASURE_WITH_UNIT(LENGTH_MEASURE(0.001),#7350,
'DISTANCE_ACCURACY_VALUE',
'Maximum model space distance between geometric entities at asserted c
onnectivities');
#7323=UNCERTAINTY_MEASURE_WITH_UNIT(LENGTH_MEASURE(0.001),#7350,
'DISTANCE_ACCURACY_VALUE',
'Maximum model space distance between geometric entities at asserted c
onnectivities');
#7324=UNCERTAINTY_MEASURE_WITH_UNIT(LENGTH_MEASURE(0.001),#7350,
'DISTANCE_ACCURACY_VALUE',
'Maximum model space distance between geometric entities at asserted c
onnectivities');
#7325=(
GEOMETRIC_REPRESENTATION_CONTEXT(3)
GLOBAL_UNCERTAINTY_ASSIGNED_CONTEXT((#7300))
GLOBAL_UNIT_ASSIGNED_CONTEXT((#7350,#7352,#7353))
REPRESENTATION_CONTEXT('','3D')
);
#7326=(
GEOMETRIC_REPRESENTATION_CONTEXT(3)
GLOBAL_UNCERTAINTY_ASSIGNED_CONTEXT((#7301))
GLOBAL_UNIT_ASSIGNED_CONTEXT((#7350,#7352,#7353))
REPRESENTATION_CONTEXT('','3D')
);
#7327=(
GEOMETRIC_REPRESENTATION_CONTEXT(3)
GLOBAL_UNCERTAINTY_ASSIGNED_CONTEXT((#7302))
GLOBAL_UNIT_ASSIGNED_CONTEXT((#7350,#7352,#7353))
REPRESENTATION_CONTEXT('','3D')
);
#7328=(
GEOMETRIC_REPRESENTATION_CONTEXT(3)
GLOBAL_UNCERTAINTY_ASSIGNED_CONTEXT((#7303))
GLOBAL_UNIT_ASSIGNED_CONTEXT((#7350,#7352,#7353))
REPRESENTATION_CONTEXT('','3D')
);
#7329=(
GEOMETRIC_REPRESENTATION_CONTEXT(3)
GLOBAL_UNCERTAINTY_ASSIGNED_CONTEXT((#7304))
GLOBAL_UNIT_ASSIGNED_CONTEXT((#7350,#7352,#7353))
REPRESENTATION_CONTEXT('','3D')
);
#7330=(
GEOMETRIC_REPRESENTATION_CONTEXT(3)
GLOBAL_UNCERTAINTY_ASSIGNED_CONTEXT((#7305))
GLOBAL_UNIT_ASSIGNED_CONTEXT((#7350,#7352,#7353))
REPRESENTATION_CONTEXT('','3D')
);
#7331=(
GEOMETRIC_REPRESENTATION_CONTEXT(3)
GLOBAL_UNCERTAINTY_ASSIGNED_CONTEXT((#7306))
GLOBAL_UNIT_ASSIGNED_CONTEXT((#7350,#7352,#7353))
REPRESENTATION_CONTEXT('','3D')
);
#7332=(
GEOMETRIC_REPRESENTATION_CONTEXT(3)
GLOBAL_UNCERTAINTY_ASSIGNED_CONTEXT((#7307))
GLOBAL_UNIT_ASSIGNED_CONTEXT((#7350,#7352,#7353))
REPRESENTATION_CONTEXT('','3D')
);
#7333=(
GEOMETRIC_REPRESENTATION_CONTEXT(3)
GLOBAL_UNCERTAINTY_ASSIGNED_CONTEXT((#7308))
GLOBAL_UNIT_ASSIGNED_CONTEXT((#7350,#7352,#7353))
REPRESENTATION_CONTEXT('','3D')
);
#7334=(
GEOMETRIC_REPRESENTATION_CONTEXT(3)
GLOBAL_UNCERTAINTY_ASSIGNED_CONTEXT((#7309))
GLOBAL_UNIT_ASSIGNED_CONTEXT((#7350,#7352,#7353))
REPRESENTATION_CONTEXT('','3D')
);
#7335=(
GEOMETRIC_REPRESENTATION_CONTEXT(3)
GLOBAL_UNCERTAINTY_ASSIGNED_CONTEXT((#7310))
GLOBAL_UNIT_ASSIGNED_CONTEXT((#7350,#7352,#7353))
REPRESENTATION_CONTEXT('','3D')
);
#7336=(
GEOMETRIC_REPRESENTATION_CONTEXT(3)
GLOBAL_UNCERTAINTY_ASSIGNED_CONTEXT((#7311))
GLOBAL_UNIT_ASSIGNED_CONTEXT((#7350,#7352,#7353))
REPRESENTATION_CONTEXT('','3D')
);
#7337=(
GEOMETRIC_REPRESENTATION_CONTEXT(3)
GLOBAL_UNCERTAINTY_ASSIGNED_CONTEXT((#7312))
GLOBAL_UNIT_ASSIGNED_CONTEXT((#7350,#7352,#7353))
REPRESENTATION_CONTEXT('','3D')
);
#7338=(
GEOMETRIC_REPRESENTATION_CONTEXT(3)
GLOBAL_UNCERTAINTY_ASSIGNED_CONTEXT((#7313))
GLOBAL_UNIT_ASSIGNED_CONTEXT((#7350,#7352,#7353))
REPRESENTATION_CONTEXT('','3D')
);
#7339=(
GEOMETRIC_REPRESENTATION_CONTEXT(3)
GLOBAL_UNCERTAINTY_ASSIGNED_CONTEXT((#7314))
GLOBAL_UNIT_ASSIGNED_CONTEXT((#7350,#7352,#7353))
REPRESENTATION_CONTEXT('','3D')
);
#7340=(
GEOMETRIC_REPRESENTATION_CONTEXT(3)
GLOBAL_UNCERTAINTY_ASSIGNED_CONTEXT((#7315))
GLOBAL_UNIT_ASSIGNED_CONTEXT((#7350,#7352,#7353))
REPRESENTATION_CONTEXT('','3D')
);
#7341=(
GEOMETRIC_REPRESENTATION_CONTEXT(3)
GLOBAL_UNCERTAINTY_ASSIGNED_CONTEXT((#7316))
GLOBAL_UNIT_ASSIGNED_CONTEXT((#7350,#7352,#7353))
REPRESENTATION_CONTEXT('','3D')
);
#7342=(
GEOMETRIC_REPRESENTATION_CONTEXT(3)
GLOBAL_UNCERTAINTY_ASSIGNED_CONTEXT((#7317))
GLOBAL_UNIT_ASSIGNED_CONTEXT((#7350,#7352,#7353))
REPRESENTATION_CONTEXT('','3D')
);
#7343=(
GEOMETRIC_REPRESENTATION_CONTEXT(3)
GLOBAL_UNCERTAINTY_ASSIGNED_CONTEXT((#7318))
GLOBAL_UNIT_ASSIGNED_CONTEXT((#7350,#7352,#7353))
REPRESENTATION_CONTEXT('','3D')
);
#7344=(
GEOMETRIC_REPRESENTATION_CONTEXT(3)
GLOBAL_UNCERTAINTY_ASSIGNED_CONTEXT((#7319))
GLOBAL_UNIT_ASSIGNED_CONTEXT((#7350,#7352,#7353))
REPRESENTATION_CONTEXT('','3D')
);
#7345=(
GEOMETRIC_REPRESENTATION_CONTEXT(3)
GLOBAL_UNCERTAINTY_ASSIGNED_CONTEXT((#7320))
GLOBAL_UNIT_ASSIGNED_CONTEXT((#7350,#7352,#7353))
REPRESENTATION_CONTEXT('','3D')
);
#7346=(
GEOMETRIC_REPRESENTATION_CONTEXT(3)
GLOBAL_UNCERTAINTY_ASSIGNED_CONTEXT((#7321))
GLOBAL_UNIT_ASSIGNED_CONTEXT((#7350,#7352,#7353))
REPRESENTATION_CONTEXT('','3D')
);
#7347=(
GEOMETRIC_REPRESENTATION_CONTEXT(3)
GLOBAL_UNCERTAINTY_ASSIGNED_CONTEXT((#7322))
GLOBAL_UNIT_ASSIGNED_CONTEXT((#7350,#7352,#7353))
REPRESENTATION_CONTEXT('','3D')
);
#7348=(
GEOMETRIC_REPRESENTATION_CONTEXT(3)
GLOBAL_UNCERTAINTY_ASSIGNED_CONTEXT((#7323))
GLOBAL_UNIT_ASSIGNED_CONTEXT((#7350,#7352,#7353))
REPRESENTATION_CONTEXT('','3D')
);
#7349=(
GEOMETRIC_REPRESENTATION_CONTEXT(3)
GLOBAL_UNCERTAINTY_ASSIGNED_CONTEXT((#7324))
GLOBAL_UNIT_ASSIGNED_CONTEXT((#7350,#7352,#7353))
REPRESENTATION_CONTEXT('','3D')
);
#7350=(
LENGTH_UNIT()
NAMED_UNIT(*)
SI_UNIT(.CENTI.,.METRE.)
);
#7351=(
LENGTH_UNIT()
NAMED_UNIT(*)
SI_UNIT($,.METRE.)
);
#7352=(
NAMED_UNIT(*)
PLANE_ANGLE_UNIT()
SI_UNIT($,.RADIAN.)
);
#7353=(
NAMED_UNIT(*)
SI_UNIT($,.STERADIAN.)
SOLID_ANGLE_UNIT()
);
#7354=SHAPE_DEFINITION_REPRESENTATION(#7378,#7441);
#7355=SHAPE_DEFINITION_REPRESENTATION(#7379,#7442);
#7356=SHAPE_DEFINITION_REPRESENTATION(#7380,#7443);
#7357=SHAPE_DEFINITION_REPRESENTATION(#7381,#7444);
#7358=SHAPE_DEFINITION_REPRESENTATION(#7382,#7445);
#7359=SHAPE_DEFINITION_REPRESENTATION(#7383,#7446);
#7360=SHAPE_DEFINITION_REPRESENTATION(#7384,#7447);
#7361=SHAPE_DEFINITION_REPRESENTATION(#7385,#7448);
#7362=SHAPE_DEFINITION_REPRESENTATION(#7386,#7449);
#7363=SHAPE_DEFINITION_REPRESENTATION(#7387,#7450);
#7364=SHAPE_DEFINITION_REPRESENTATION(#7388,#7451);
#7365=SHAPE_DEFINITION_REPRESENTATION(#7389,#7452);
#7366=SHAPE_DEFINITION_REPRESENTATION(#7390,#7453);
#7367=SHAPE_DEFINITION_REPRESENTATION(#7391,#7454);
#7368=SHAPE_DEFINITION_REPRESENTATION(#7392,#7455);
#7369=SHAPE_DEFINITION_REPRESENTATION(#7393,#7456);
#7370=SHAPE_DEFINITION_REPRESENTATION(#7394,#7457);
#7371=SHAPE_DEFINITION_REPRESENTATION(#7397,#7458);
#7372=SHAPE_DEFINITION_REPRESENTATION(#7398,#7459);
#7373=SHAPE_DEFINITION_REPRESENTATION(#7399,#7460);
#7374=SHAPE_DEFINITION_REPRESENTATION(#7400,#7461);
#7375=SHAPE_DEFINITION_REPRESENTATION(#7401,#7462);
#7376=SHAPE_DEFINITION_REPRESENTATION(#7402,#7463);
#7377=SHAPE_DEFINITION_REPRESENTATION(#7403,#7464);
#7378=PRODUCT_DEFINITION_SHAPE('',$,#7466);
#7379=PRODUCT_DEFINITION_SHAPE('',$,#7467);
#7380=PRODUCT_DEFINITION_SHAPE('',$,#7468);
#7381=PRODUCT_DEFINITION_SHAPE('',$,#7469);
#7382=PRODUCT_DEFINITION_SHAPE('',$,#7470);
#7383=PRODUCT_DEFINITION_SHAPE('',$,#7471);
#7384=PRODUCT_DEFINITION_SHAPE('',$,#7472);
#7385=PRODUCT_DEFINITION_SHAPE('',$,#7473);
#7386=PRODUCT_DEFINITION_SHAPE('',$,#7474);
#7387=PRODUCT_DEFINITION_SHAPE('',$,#7475);
#7388=PRODUCT_DEFINITION_SHAPE('',$,#7476);
#7389=PRODUCT_DEFINITION_SHAPE('',$,#7477);
#7390=PRODUCT_DEFINITION_SHAPE('',$,#7478);
#7391=PRODUCT_DEFINITION_SHAPE('',$,#7479);
#7392=PRODUCT_DEFINITION_SHAPE('',$,#7480);
#7393=PRODUCT_DEFINITION_SHAPE('',$,#7481);
#7394=PRODUCT_DEFINITION_SHAPE('',$,#7482);
#7395=PRODUCT_DEFINITION_SHAPE($,$,#128);
#7396=PRODUCT_DEFINITION_SHAPE($,$,#129);
#7397=PRODUCT_DEFINITION_SHAPE('',$,#7483);
#7398=PRODUCT_DEFINITION_SHAPE('',$,#7484);
#7399=PRODUCT_DEFINITION_SHAPE('',$,#7485);
#7400=PRODUCT_DEFINITION_SHAPE('',$,#7486);
#7401=PRODUCT_DEFINITION_SHAPE('',$,#7487);
#7402=PRODUCT_DEFINITION_SHAPE('',$,#7488);
#7403=PRODUCT_DEFINITION_SHAPE('',$,#7489);
#7404=PRODUCT_DEFINITION_SHAPE($,$,#130);
#7405=PRODUCT_DEFINITION_SHAPE($,$,#131);
#7406=PRODUCT_DEFINITION_SHAPE($,$,#132);
#7407=PRODUCT_DEFINITION_SHAPE($,$,#133);
#7408=PRODUCT_DEFINITION_SHAPE($,$,#134);
#7409=PRODUCT_DEFINITION_SHAPE($,$,#135);
#7410=PRODUCT_DEFINITION_SHAPE($,$,#136);
#7411=PRODUCT_DEFINITION_SHAPE($,$,#137);
#7412=PRODUCT_DEFINITION_SHAPE($,$,#138);
#7413=PRODUCT_DEFINITION_SHAPE($,$,#139);
#7414=PRODUCT_DEFINITION_SHAPE($,$,#140);
#7415=PRODUCT_DEFINITION_SHAPE($,$,#141);
#7416=PRODUCT_DEFINITION_SHAPE($,$,#142);
#7417=PRODUCT_DEFINITION_SHAPE($,$,#143);
#7418=PRODUCT_DEFINITION_SHAPE($,$,#144);
#7419=PRODUCT_DEFINITION_SHAPE($,$,#145);
#7420=PRODUCT_DEFINITION_SHAPE($,$,#146);
#7421=PRODUCT_DEFINITION_SHAPE($,$,#147);
#7422=PRODUCT_DEFINITION_SHAPE($,$,#148);
#7423=PRODUCT_DEFINITION_SHAPE($,$,#149);
#7424=PRODUCT_DEFINITION_SHAPE($,$,#150);
#7425=PRODUCT_DEFINITION_SHAPE($,$,#151);
#7426=PRODUCT_DEFINITION_SHAPE($,$,#152);
#7427=PRODUCT_DEFINITION_SHAPE($,$,#153);
#7428=PRODUCT_DEFINITION_SHAPE($,$,#154);
#7429=PRODUCT_DEFINITION_SHAPE($,$,#155);
#7430=PRODUCT_DEFINITION_SHAPE($,$,#156);
#7431=PRODUCT_DEFINITION_SHAPE($,$,#157);
#7432=PRODUCT_DEFINITION_SHAPE($,$,#158);
#7433=PRODUCT_DEFINITION_SHAPE($,$,#159);
#7434=PRODUCT_DEFINITION_SHAPE($,$,#160);
#7435=PRODUCT_DEFINITION_SHAPE($,$,#161);
#7436=PRODUCT_DEFINITION_SHAPE($,$,#162);
#7437=PRODUCT_DEFINITION_SHAPE($,$,#163);
#7438=PRODUCT_DEFINITION_SHAPE($,$,#164);
#7439=PRODUCT_DEFINITION_SHAPE($,$,#165);
#7440=PRODUCT_DEFINITION_SHAPE($,$,#166);
#7441=SHAPE_REPRESENTATION('',(#4207,#4705,#4706),#7325);
#7442=SHAPE_REPRESENTATION('',(#4208,#4670,#4671,#4672,#4673,#4674,#4675,
#4676,#4677,#4678,#4679,#4680,#4681,#4682,#4683,#4684,#4685,#4686,#4687,
#4688,#4689,#4690,#4691,#4692,#4693,#4694,#4695,#4696,#4697),#7326);
#7443=SHAPE_REPRESENTATION('',(#4209),#7327);
#7444=SHAPE_REPRESENTATION('',(#4228),#7328);
#7445=SHAPE_REPRESENTATION('',(#4293),#7329);
#7446=SHAPE_REPRESENTATION('',(#4320),#7330);
#7447=SHAPE_REPRESENTATION('',(#4345),#7331);
#7448=SHAPE_REPRESENTATION('',(#4372),#7332);
#7449=SHAPE_REPRESENTATION('',(#4397),#7333);
#7450=SHAPE_REPRESENTATION('',(#4406),#7334);
#7451=SHAPE_REPRESENTATION('',(#4415),#7335);
#7452=SHAPE_REPRESENTATION('',(#4424),#7336);
#7453=SHAPE_REPRESENTATION('',(#4446),#7337);
#7454=SHAPE_REPRESENTATION('',(#4493),#7338);
#7455=SHAPE_REPRESENTATION('',(#4519,#4569,#4570),#7339);
#7456=SHAPE_REPRESENTATION('',(#4520),#7340);
#7457=SHAPE_REPRESENTATION('',(#4552),#7341);
#7458=SHAPE_REPRESENTATION('',(#4571,#4698,#4699,#4700,#4701,#4702,#4703,
#4704),#7342);
#7459=SHAPE_REPRESENTATION('',(#4572),#7343);
#7460=SHAPE_REPRESENTATION('',(#4586),#7344);
#7461=SHAPE_REPRESENTATION('',(#4600),#7345);
#7462=SHAPE_REPRESENTATION('',(#4613),#7346);
#7463=SHAPE_REPRESENTATION('',(#4627),#7347);
#7464=SHAPE_REPRESENTATION('',(#4644),#7348);
#7465=PRODUCT_DEFINITION_CONTEXT('part definition',#7539,'design');
#7466=PRODUCT_DEFINITION('PAT-103',
'PAT-103',#7490,#7465);
#7467=PRODUCT_DEFINITION('Bearing housing and clamp',
'Bearing housing and clamp',#7491,#7465);
#7468=PRODUCT_DEFINITION('Base','Base',#7492,#7465);
#7469=PRODUCT_DEFINITION('Bushing tube','Bushing tube',#7493,#7465);
#7470=PRODUCT_DEFINITION('Lower tube clamp','Lower tube clamp',#7494,#7465);
#7471=PRODUCT_DEFINITION('Upper tube clamp','Upper tube clamp',#7495,#7465);
#7472=PRODUCT_DEFINITION('Lower tube clamp (1)','Lower tube clamp (1)',#7496,
#7465);
#7473=PRODUCT_DEFINITION('Upper tube clamp (1)','Upper tube clamp (1)',#7497,
#7465);
#7474=PRODUCT_DEFINITION('Inner bushing spacer','Inner bushing spacer',
#7498,#7465);
#7475=PRODUCT_DEFINITION('End bushing spacer','End bushing spacer',#7499,
#7465);
#7476=PRODUCT_DEFINITION('End bushing spacer (1)',
'End bushing spacer (1)',#7500,#7465);
#7477=PRODUCT_DEFINITION('Rear retainer','Rear retainer',#7501,#7465);
#7478=PRODUCT_DEFINITION('Split locking cap','Split locking cap',#7502,
#7465);
#7479=PRODUCT_DEFINITION('Cap Screw - M5x20','Cap Screw - M5x20',#7503,
#7465);
#7480=PRODUCT_DEFINITION('Linear Ball Bushing - 12 x 21 x 30 mm',
'Linear Ball Bushing - 12 x 21 x 30 mm',#7504,#7465);
#7481=PRODUCT_DEFINITION('Steel sleeve','Steel sleeve',#7505,#7465);
#7482=PRODUCT_DEFINITION('Ball retainer (plastic)',
'Ball retainer (plastic)',#7506,#7465);
#7483=PRODUCT_DEFINITION('Sliding shaft','Sliding shaft',#7507,#7465);
#7484=PRODUCT_DEFINITION('Travel stop collar','Travel stop collar',#7508,
#7465);
#7485=PRODUCT_DEFINITION('Travel stop collar (1)',
'Travel stop collar (1)',#7509,#7465);
#7486=PRODUCT_DEFINITION('Pull knob','Pull knob',#7510,#7465);
#7487=PRODUCT_DEFINITION(
'Precision Shaft - 12 mm Diameter, 300 mm Long',
'Precision Shaft - 12 mm Diameter, 300 mm Long',#7511,#7465);
#7488=PRODUCT_DEFINITION('Socket Set Screw - M5x8',
'Socket Set Screw - M5x8',#7512,#7465);
#7489=PRODUCT_DEFINITION('Cap Screw - M4x16','Cap Screw - M4x16',#7513,
#7465);
#7490=PRODUCT_DEFINITION_FORMATION('',$,#7541);
#7491=PRODUCT_DEFINITION_FORMATION('',$,#7542);
#7492=PRODUCT_DEFINITION_FORMATION('',$,#7543);
#7493=PRODUCT_DEFINITION_FORMATION('',$,#7544);
#7494=PRODUCT_DEFINITION_FORMATION('',$,#7545);
#7495=PRODUCT_DEFINITION_FORMATION('',$,#7546);
#7496=PRODUCT_DEFINITION_FORMATION('',$,#7547);
#7497=PRODUCT_DEFINITION_FORMATION('',$,#7548);
#7498=PRODUCT_DEFINITION_FORMATION('',$,#7549);
#7499=PRODUCT_DEFINITION_FORMATION('',$,#7550);
#7500=PRODUCT_DEFINITION_FORMATION('',$,#7551);
#7501=PRODUCT_DEFINITION_FORMATION('',$,#7552);
#7502=PRODUCT_DEFINITION_FORMATION('',$,#7553);
#7503=PRODUCT_DEFINITION_FORMATION('',$,#7554);
#7504=PRODUCT_DEFINITION_FORMATION('',$,#7555);
#7505=PRODUCT_DEFINITION_FORMATION('',$,#7556);
#7506=PRODUCT_DEFINITION_FORMATION('',$,#7557);
#7507=PRODUCT_DEFINITION_FORMATION('',$,#7558);
#7508=PRODUCT_DEFINITION_FORMATION('',$,#7559);
#7509=PRODUCT_DEFINITION_FORMATION('',$,#7560);
#7510=PRODUCT_DEFINITION_FORMATION('',$,#7561);
#7511=PRODUCT_DEFINITION_FORMATION('',$,#7562);
#7512=PRODUCT_DEFINITION_FORMATION('',$,#7563);
#7513=PRODUCT_DEFINITION_FORMATION('',$,#7564);
#7514=PRODUCT_RELATED_PRODUCT_CATEGORY('PAT-103','PAT-103',(#7541));
#7515=PRODUCT_RELATED_PRODUCT_CATEGORY('Bearing housing and clamp',
'Bearing housing and clamp',(#7542));
#7516=PRODUCT_RELATED_PRODUCT_CATEGORY('Base','Base',(#7543));
#7517=PRODUCT_RELATED_PRODUCT_CATEGORY('Bushing tube','Bushing tube',(#7544));
#7518=PRODUCT_RELATED_PRODUCT_CATEGORY('Lower tube clamp',
'Lower tube clamp',(#7545));
#7519=PRODUCT_RELATED_PRODUCT_CATEGORY('Upper tube clamp',
'Upper tube clamp',(#7546));
#7520=PRODUCT_RELATED_PRODUCT_CATEGORY('Lower tube clamp (1)',
'Lower tube clamp (1)',(#7547));
#7521=PRODUCT_RELATED_PRODUCT_CATEGORY('Upper tube clamp (1)',
'Upper tube clamp (1)',(#7548));
#7522=PRODUCT_RELATED_PRODUCT_CATEGORY('Inner bushing spacer',
'Inner bushing spacer',(#7549));
#7523=PRODUCT_RELATED_PRODUCT_CATEGORY('End bushing spacer',
'End bushing spacer',(#7550));
#7524=PRODUCT_RELATED_PRODUCT_CATEGORY('End bushing spacer (1)',
'End bushing spacer (1)',(#7551));
#7525=PRODUCT_RELATED_PRODUCT_CATEGORY('Rear retainer','Rear retainer',
(#7552));
#7526=PRODUCT_RELATED_PRODUCT_CATEGORY('Split locking cap',
'Split locking cap',(#7553));
#7527=PRODUCT_RELATED_PRODUCT_CATEGORY('Cap Screw - M5x20',
'Cap Screw - M5x20',(#7554));
#7528=PRODUCT_RELATED_PRODUCT_CATEGORY(
'Linear Ball Bushing - 12 x 21 x 30 mm',
'Linear Ball Bushing - 12 x 21 x 30 mm',(#7555));
#7529=PRODUCT_RELATED_PRODUCT_CATEGORY('Steel sleeve','Steel sleeve',(#7556));
#7530=PRODUCT_RELATED_PRODUCT_CATEGORY('Ball retainer (plastic)',
'Ball retainer (plastic)',(#7557));
#7531=PRODUCT_RELATED_PRODUCT_CATEGORY('Sliding shaft','Sliding shaft',
(#7558));
#7532=PRODUCT_RELATED_PRODUCT_CATEGORY('Travel stop collar',
'Travel stop collar',(#7559));
#7533=PRODUCT_RELATED_PRODUCT_CATEGORY('Travel stop collar (1)',
'Travel stop collar (1)',(#7560));
#7534=PRODUCT_RELATED_PRODUCT_CATEGORY('Pull knob','Pull knob',(#7561));
#7535=PRODUCT_RELATED_PRODUCT_CATEGORY(
'Precision Shaft - 12 mm Diameter, 300 mm Long',
'Precision Shaft - 12 mm Diameter, 300 mm Long',(#7562));
#7536=PRODUCT_RELATED_PRODUCT_CATEGORY('Socket Set Screw - M5x8',
'Socket Set Screw - M5x8',(#7563));
#7537=PRODUCT_RELATED_PRODUCT_CATEGORY('Cap Screw - M4x16',
'Cap Screw - M4x16',(#7564));
#7538=APPLICATION_PROTOCOL_DEFINITION('international standard',
'automotive_design',2009,#7539);
#7539=APPLICATION_CONTEXT(
'Core Data for Automotive Mechanical Design Process');
#7540=PRODUCT_CONTEXT('part definition',#7539,'mechanical');
#7541=PRODUCT('PAT-103','PAT-103',
'PAT-103',(#7540));
#7542=PRODUCT('Bearing housing and clamp','Bearing housing and clamp',
'Bearing housing and clamp',(#7540));
#7543=PRODUCT('Base','Base','Base',(#7540));
#7544=PRODUCT('Bushing tube','Bushing tube','Bushing tube',(#7540));
#7545=PRODUCT('Lower tube clamp','Lower tube clamp','Lower tube clamp',
(#7540));
#7546=PRODUCT('Upper tube clamp','Upper tube clamp','Upper tube clamp',
(#7540));
#7547=PRODUCT('Lower tube clamp (1)','Lower tube clamp (1)',
'Lower tube clamp (1)',(#7540));
#7548=PRODUCT('Upper tube clamp (1)','Upper tube clamp (1)',
'Upper tube clamp (1)',(#7540));
#7549=PRODUCT('Inner bushing spacer','Inner bushing spacer',
'Inner bushing spacer',(#7540));
#7550=PRODUCT('End bushing spacer','End bushing spacer',
'End bushing spacer',(#7540));
#7551=PRODUCT('End bushing spacer (1)','End bushing spacer (1)',
'End bushing spacer (1)',(#7540));
#7552=PRODUCT('Rear retainer','Rear retainer','Rear retainer',(#7540));
#7553=PRODUCT('Split locking cap','Split locking cap',
'Split locking cap',(#7540));
#7554=PRODUCT('Cap Screw - M5x20','Cap Screw - M5x20',
'Cap Screw - M5x20',(#7540));
#7555=PRODUCT('Linear Ball Bushing - 12 x 21 x 30 mm',
'Linear Ball Bushing - 12 x 21 x 30 mm',
'Linear Ball Bushing - 12 x 21 x 30 mm',(#7540));
#7556=PRODUCT('Steel sleeve','Steel sleeve','Steel sleeve',(#7540));
#7557=PRODUCT('Ball retainer (plastic)','Ball retainer (plastic)',
'Ball retainer (plastic)',(#7540));
#7558=PRODUCT('Sliding shaft','Sliding shaft','Sliding shaft',(#7540));
#7559=PRODUCT('Travel stop collar','Travel stop collar',
'Travel stop collar',(#7540));
#7560=PRODUCT('Travel stop collar (1)','Travel stop collar (1)',
'Travel stop collar (1)',(#7540));
#7561=PRODUCT('Pull knob','Pull knob','Pull knob',(#7540));
#7562=PRODUCT('Precision Shaft - 12 mm Diameter, 300 mm Long',
'Precision Shaft - 12 mm Diameter, 300 mm Long',
'Precision Shaft - 12 mm Diameter, 300 mm Long',(#7540));
#7563=PRODUCT('Socket Set Screw - M5x8','Socket Set Screw - M5x8',
'Socket Set Screw - M5x8',(#7540));
#7564=PRODUCT('Cap Screw - M4x16','Cap Screw - M4x16',
'Cap Screw - M4x16',(#7540));
#7565=PRESENTATION_STYLE_ASSIGNMENT((#7570));
#7566=PRESENTATION_STYLE_ASSIGNMENT((#7571));
#7567=PRESENTATION_STYLE_ASSIGNMENT((#7572));
#7568=PRESENTATION_STYLE_ASSIGNMENT((#7573));
#7569=PRESENTATION_STYLE_ASSIGNMENT((#7574));
#7570=SURFACE_STYLE_USAGE(.BOTH.,#7575);
#7571=SURFACE_STYLE_USAGE(.BOTH.,#7576);
#7572=SURFACE_STYLE_USAGE(.BOTH.,#7577);
#7573=SURFACE_STYLE_USAGE(.BOTH.,#7578);
#7574=SURFACE_STYLE_USAGE(.BOTH.,#7579);
#7575=SURFACE_SIDE_STYLE('',(#7580));
#7576=SURFACE_SIDE_STYLE('',(#7581));
#7577=SURFACE_SIDE_STYLE('',(#7582));
#7578=SURFACE_SIDE_STYLE('',(#7583));
#7579=SURFACE_SIDE_STYLE('',(#7584));
#7580=SURFACE_STYLE_FILL_AREA(#7585);
#7581=SURFACE_STYLE_FILL_AREA(#7586);
#7582=SURFACE_STYLE_FILL_AREA(#7587);
#7583=SURFACE_STYLE_FILL_AREA(#7588);
#7584=SURFACE_STYLE_FILL_AREA(#7589);
#7585=FILL_AREA_STYLE('Steel - Satin',(#7590));
#7586=FILL_AREA_STYLE('CAD Library Painted - Deep blue',(#7591));
#7587=FILL_AREA_STYLE('CAD Library Painted - Engineering blue',(#7592));
#7588=FILL_AREA_STYLE('CAD Library Painted - Steel gray',(#7593));
#7589=FILL_AREA_STYLE('CAD Library Painted - Graphite',(#7594));
#7590=FILL_AREA_STYLE_COLOUR('Steel - Satin',#7595);
#7591=FILL_AREA_STYLE_COLOUR('CAD Library Painted - Deep blue',#7596);
#7592=FILL_AREA_STYLE_COLOUR('CAD Library Painted - Engineering blue',#7597);
#7593=FILL_AREA_STYLE_COLOUR('CAD Library Painted - Steel gray',#7598);
#7594=FILL_AREA_STYLE_COLOUR('CAD Library Painted - Graphite',#7599);
#7595=COLOUR_RGB('Steel - Satin',0.627450980392157,0.627450980392157,0.627450980392157);
#7596=COLOUR_RGB('CAD Library Painted - Deep blue',0.0784313725490196,0.203921568627451,
0.349019607843137);
#7597=COLOUR_RGB('CAD Library Painted - Engineering blue',0.12156862745098,
0.356862745098039,0.6);
#7598=COLOUR_RGB('CAD Library Painted - Steel gray',0.592156862745098,0.631372549019608,
0.67843137254902);
#7599=COLOUR_RGB('CAD Library Painted - Graphite',0.168627450980392,0.192156862745098,
0.231372549019608);
#7600=COLOUR_RGB('Dark Blue',0.08,0.2,0.34);
#7601=FILL_AREA_STYLE_COLOUR('',#7600);
#7602=FILL_AREA_STYLE('',(#7601));
#7603=SURFACE_STYLE_FILL_AREA(#7602);
#7604=SURFACE_SIDE_STYLE('',(#7603));
#7605=SURFACE_STYLE_USAGE(.BOTH.,#7604);
#7606=PRESENTATION_STYLE_ASSIGNMENT((#7605));
#7607=COLOUR_RGB('Light Blue',0.38,0.62,0.78);
#7608=FILL_AREA_STYLE_COLOUR('',#7607);
#7609=FILL_AREA_STYLE('',(#7608));
#7610=SURFACE_STYLE_FILL_AREA(#7609);
#7611=SURFACE_SIDE_STYLE('',(#7610));
#7612=SURFACE_STYLE_USAGE(.BOTH.,#7611);
#7613=PRESENTATION_STYLE_ASSIGNMENT((#7612));
#7614=COLOUR_RGB('Sky Blue',0.24,0.69,0.87);
#7615=FILL_AREA_STYLE_COLOUR('',#7614);
#7616=FILL_AREA_STYLE('',(#7615));
#7617=SURFACE_STYLE_FILL_AREA(#7616);
#7618=SURFACE_SIDE_STYLE('',(#7617));
#7619=SURFACE_STYLE_USAGE(.BOTH.,#7618);
#7620=PRESENTATION_STYLE_ASSIGNMENT((#7619));
#7621=COLOUR_RGB('Grey',0.48,0.52,0.57);
#7622=FILL_AREA_STYLE_COLOUR('',#7621);
#7623=FILL_AREA_STYLE('',(#7622));
#7624=SURFACE_STYLE_FILL_AREA(#7623);
#7625=SURFACE_SIDE_STYLE('',(#7624));
#7626=SURFACE_STYLE_USAGE(.BOTH.,#7625);
#7627=PRESENTATION_STYLE_ASSIGNMENT((#7626));
#7628=COLOUR_RGB('Black',0.12,0.14,0.17);
#7629=FILL_AREA_STYLE_COLOUR('',#7628);
#7630=FILL_AREA_STYLE('',(#7629));
#7631=SURFACE_STYLE_FILL_AREA(#7630);
#7632=SURFACE_SIDE_STYLE('',(#7631));
#7633=SURFACE_STYLE_USAGE(.BOTH.,#7632);
#7634=PRESENTATION_STYLE_ASSIGNMENT((#7633));
#7635=COLOUR_RGB('Off White',0.89,0.88,0.83);
#7636=FILL_AREA_STYLE_COLOUR('',#7635);
#7637=FILL_AREA_STYLE('',(#7636));
#7638=SURFACE_STYLE_FILL_AREA(#7637);
#7639=SURFACE_SIDE_STYLE('',(#7638));
#7640=SURFACE_STYLE_USAGE(.BOTH.,#7639);
#7641=PRESENTATION_STYLE_ASSIGNMENT((#7640));
ENDSEC;
END-ISO-10303-21;
